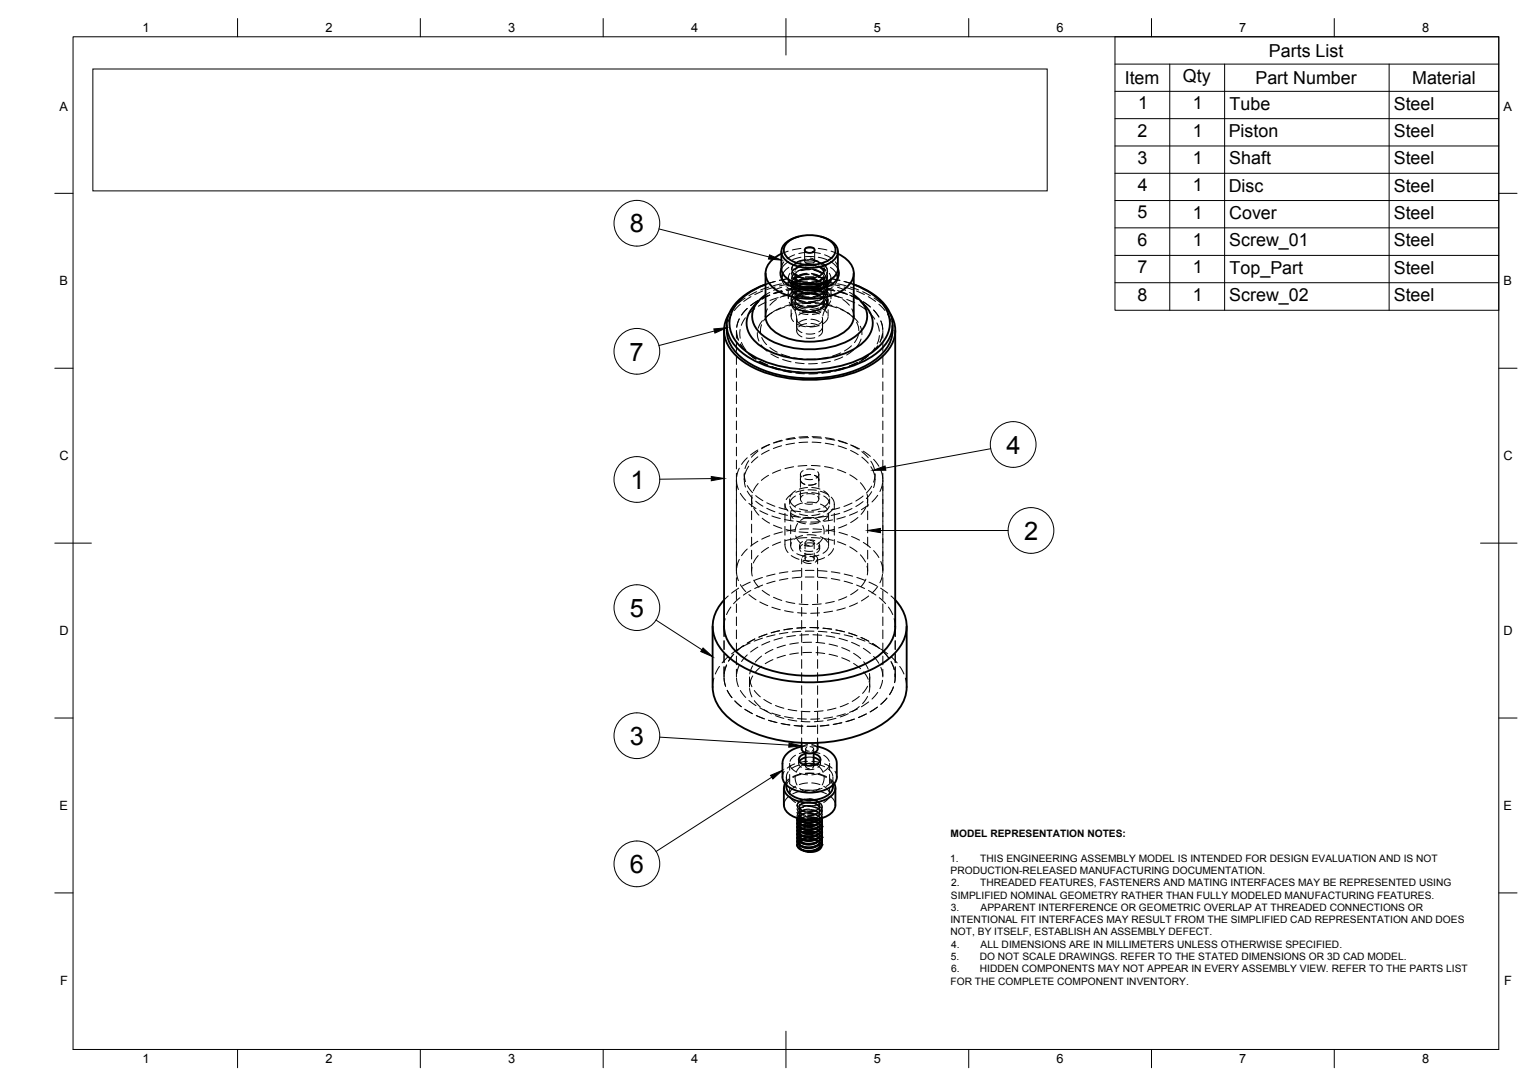
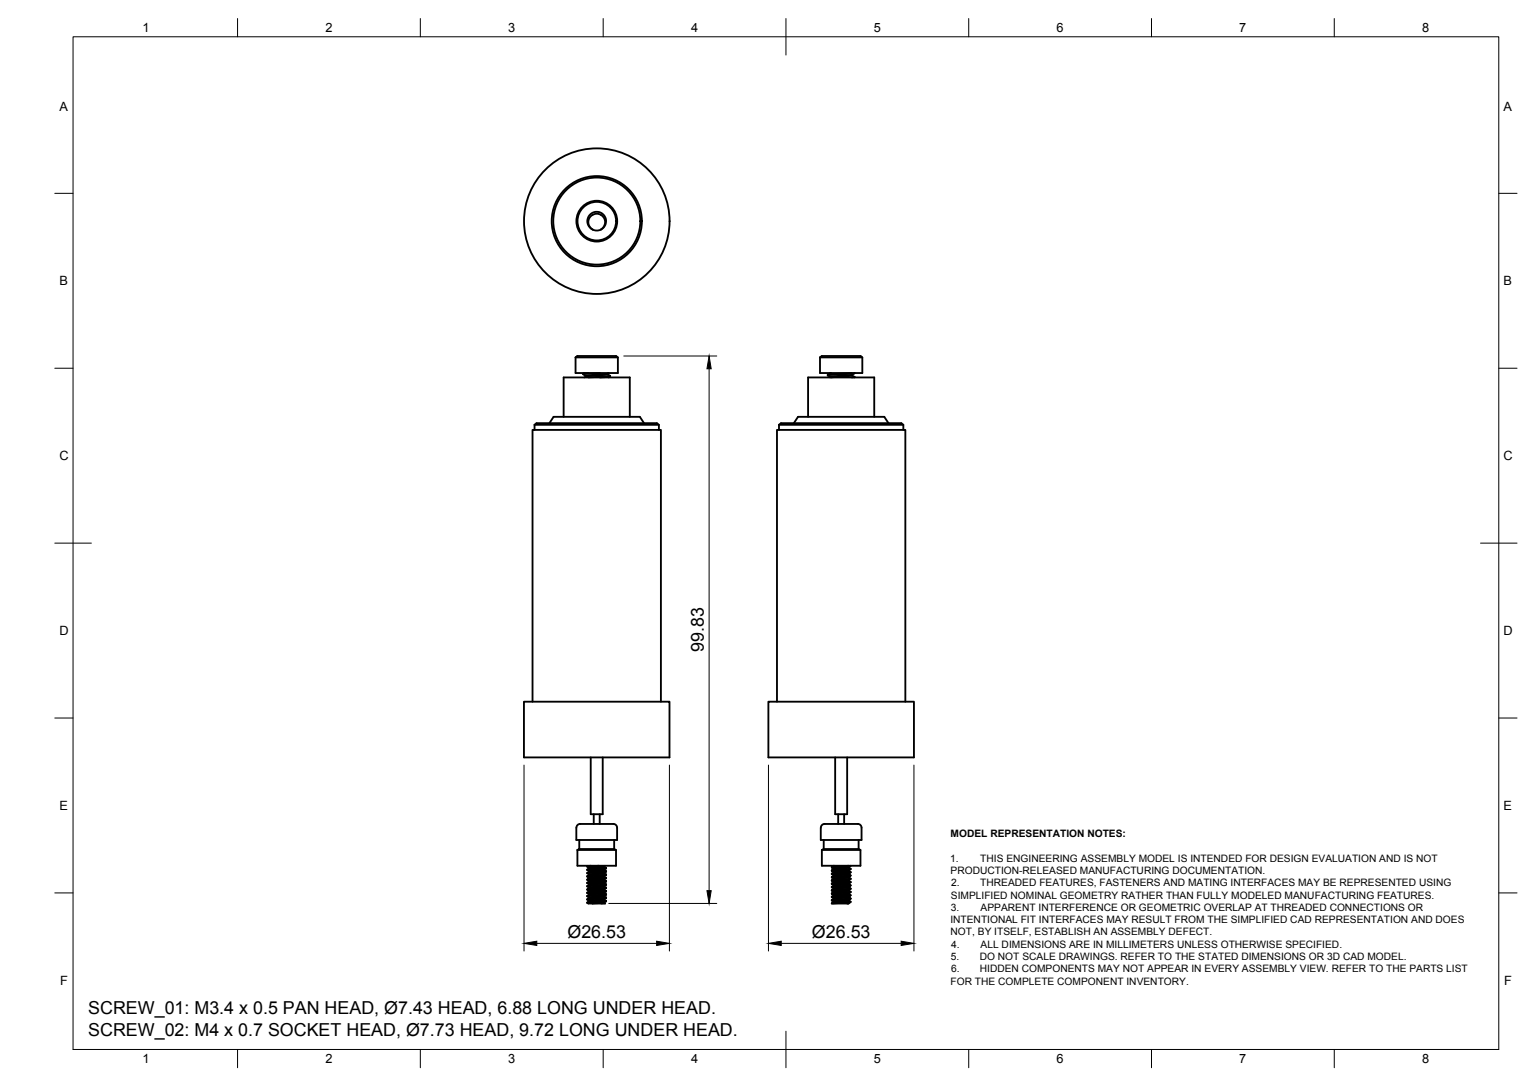
ISO-10303-21;
HEADER;
/* Generated by software containing ST-Developer
 * from STEP Tools, Inc. (www.steptools.com) 
 */

FILE_DESCRIPTION(
/* description */ (''),
/* implementation_level */ '2;1');

FILE_NAME(
/* name */ 'BR-113',
/* time_stamp */ '2026-10-04T22:56:18-07:00',
/* author */ (''),
/* organization */ (''),
/* preprocessor_version */ 'ST-DEVELOPER v20.2',
/* originating_system */ 'Autodesk Translation Framework v15.15.0.0',
/* authorisation */ '');

FILE_SCHEMA (('AUTOMOTIVE_DESIGN { 1 0 10303 214 3 1 1 }'));
ENDSEC;

DATA;
#10=MECHANICAL_DESIGN_GEOMETRIC_PRESENTATION_REPRESENTATION('',(#190,#191,
#192,#193,#194,#195,#196,#197),#14544);
#11=ITEM_DEFINED_TRANSFORMATION($,$,#1924,#2120);
#12=ITEM_DEFINED_TRANSFORMATION($,$,#1933,#2121);
#13=ITEM_DEFINED_TRANSFORMATION($,$,#1966,#2122);
#14=ITEM_DEFINED_TRANSFORMATION($,$,#1982,#2123);
#15=ITEM_DEFINED_TRANSFORMATION($,$,#1991,#2124);
#16=ITEM_DEFINED_TRANSFORMATION($,$,#2004,#2125);
#17=ITEM_DEFINED_TRANSFORMATION($,$,#2047,#2126);
#18=ITEM_DEFINED_TRANSFORMATION($,$,#2086,#2127);
#19=(
REPRESENTATION_RELATIONSHIP($,$,#14576,#14575)
REPRESENTATION_RELATIONSHIP_WITH_TRANSFORMATION(#11)
SHAPE_REPRESENTATION_RELATIONSHIP()
);
#20=(
REPRESENTATION_RELATIONSHIP($,$,#14577,#14575)
REPRESENTATION_RELATIONSHIP_WITH_TRANSFORMATION(#12)
SHAPE_REPRESENTATION_RELATIONSHIP()
);
#21=(
REPRESENTATION_RELATIONSHIP($,$,#14578,#14575)
REPRESENTATION_RELATIONSHIP_WITH_TRANSFORMATION(#13)
SHAPE_REPRESENTATION_RELATIONSHIP()
);
#22=(
REPRESENTATION_RELATIONSHIP($,$,#14579,#14575)
REPRESENTATION_RELATIONSHIP_WITH_TRANSFORMATION(#14)
SHAPE_REPRESENTATION_RELATIONSHIP()
);
#23=(
REPRESENTATION_RELATIONSHIP($,$,#14580,#14575)
REPRESENTATION_RELATIONSHIP_WITH_TRANSFORMATION(#15)
SHAPE_REPRESENTATION_RELATIONSHIP()
);
#24=(
REPRESENTATION_RELATIONSHIP($,$,#14581,#14575)
REPRESENTATION_RELATIONSHIP_WITH_TRANSFORMATION(#16)
SHAPE_REPRESENTATION_RELATIONSHIP()
);
#25=(
REPRESENTATION_RELATIONSHIP($,$,#14582,#14575)
REPRESENTATION_RELATIONSHIP_WITH_TRANSFORMATION(#17)
SHAPE_REPRESENTATION_RELATIONSHIP()
);
#26=(
REPRESENTATION_RELATIONSHIP($,$,#14583,#14575)
REPRESENTATION_RELATIONSHIP_WITH_TRANSFORMATION(#18)
SHAPE_REPRESENTATION_RELATIONSHIP()
);
#27=CONTEXT_DEPENDENT_SHAPE_REPRESENTATION(#19,#14567);
#28=CONTEXT_DEPENDENT_SHAPE_REPRESENTATION(#20,#14568);
#29=CONTEXT_DEPENDENT_SHAPE_REPRESENTATION(#21,#14569);
#30=CONTEXT_DEPENDENT_SHAPE_REPRESENTATION(#22,#14570);
#31=CONTEXT_DEPENDENT_SHAPE_REPRESENTATION(#23,#14571);
#32=CONTEXT_DEPENDENT_SHAPE_REPRESENTATION(#24,#14572);
#33=CONTEXT_DEPENDENT_SHAPE_REPRESENTATION(#25,#14573);
#34=CONTEXT_DEPENDENT_SHAPE_REPRESENTATION(#26,#14574);
#35=NEXT_ASSEMBLY_USAGE_OCCURRENCE('Tube:1','Tube:1','Tube:1',#14585,#14586,
'Tube:1');
#36=NEXT_ASSEMBLY_USAGE_OCCURRENCE('Piston:1','Piston:1','Piston:1',#14585,
#14587,'Piston:1');
#37=NEXT_ASSEMBLY_USAGE_OCCURRENCE('Shaft:1','Shaft:1','Shaft:1',#14585,
#14588,'Shaft:1');
#38=NEXT_ASSEMBLY_USAGE_OCCURRENCE('Disc:1','Disc:1','Disc:1',#14585,#14589,
'Disc:1');
#39=NEXT_ASSEMBLY_USAGE_OCCURRENCE('Cover:1','Cover:1','Cover:1',#14585,
#14590,'Cover:1');
#40=NEXT_ASSEMBLY_USAGE_OCCURRENCE('Screw_01:1','Screw_01:1',
'Screw_01:1',#14585,#14591,'Screw_01:1');
#41=NEXT_ASSEMBLY_USAGE_OCCURRENCE('Top_Part:1','Top_Part:1',
'Top_Part:1',#14585,#14592,'Top_Part:1');
#42=NEXT_ASSEMBLY_USAGE_OCCURRENCE('Screw_02:1','Screw_02:1',
'Screw_02:1',#14585,#14593,'Screw_02:1');
#43=CONICAL_SURFACE('',#2029,3.34979916874976,1.09810780243133);
#44=CONICAL_SURFACE('',#2051,6.94221583892671,0.735432745767903);
#45=CONICAL_SURFACE('',#2055,9.77637943942299,0.712897062744303);
#46=CONICAL_SURFACE('',#2061,11.1537701181833,0.893668754257897);
#47=CONICAL_SURFACE('',#2065,8.2465180845384,0.582247271411204);
#48=CONICAL_SURFACE('',#2073,3.90337928524842,0.252845151189765);
#49=CONICAL_SURFACE('',#2083,2.14952775522097,1.03539162387167);
#50=CONICAL_SURFACE('',#2110,3.70051543670999,0.906750163968186);
#51=B_SPLINE_SURFACE_WITH_KNOTS('',3,3,((#7599,#7600,#7601,#7602,#7603,
#7604,#7605,#7606,#7607,#7608,#7609,#7610,#7611,#7612,#7613,#7614,#7615,
#7616,#7617,#7618,#7619,#7620,#7621,#7622,#7623,#7624,#7625,#7626,#7627,
#7628,#7629,#7630,#7631,#7632,#7633,#7634,#7635,#7636,#7637,#7638,#7639,
#7640,#7641,#7642,#7643,#7644,#7645,#7646,#7647,#7648,#7649,#7650,#7651,
#7652,#7653,#7654,#7655,#7656,#7657,#7658,#7659,#7660,#7661,#7662,#7663,
#7664,#7665,#7666,#7667,#7668,#7669,#7670,#7671,#7672,#7673,#7674,#7675,
#7676),(#7677,#7678,#7679,#7680,#7681,#7682,#7683,#7684,#7685,#7686,#7687,
#7688,#7689,#7690,#7691,#7692,#7693,#7694,#7695,#7696,#7697,#7698,#7699,
#7700,#7701,#7702,#7703,#7704,#7705,#7706,#7707,#7708,#7709,#7710,#7711,
#7712,#7713,#7714,#7715,#7716,#7717,#7718,#7719,#7720,#7721,#7722,#7723,
#7724,#7725,#7726,#7727,#7728,#7729,#7730,#7731,#7732,#7733,#7734,#7735,
#7736,#7737,#7738,#7739,#7740,#7741,#7742,#7743,#7744,#7745,#7746,#7747,
#7748,#7749,#7750,#7751,#7752,#7753,#7754),(#7755,#7756,#7757,#7758,#7759,
#7760,#7761,#7762,#7763,#7764,#7765,#7766,#7767,#7768,#7769,#7770,#7771,
#7772,#7773,#7774,#7775,#7776,#7777,#7778,#7779,#7780,#7781,#7782,#7783,
#7784,#7785,#7786,#7787,#7788,#7789,#7790,#7791,#7792,#7793,#7794,#7795,
#7796,#7797,#7798,#7799,#7800,#7801,#7802,#7803,#7804,#7805,#7806,#7807,
#7808,#7809,#7810,#7811,#7812,#7813,#7814,#7815,#7816,#7817,#7818,#7819,
#7820,#7821,#7822,#7823,#7824,#7825,#7826,#7827,#7828,#7829,#7830,#7831,
#7832),(#7833,#7834,#7835,#7836,#7837,#7838,#7839,#7840,#7841,#7842,#7843,
#7844,#7845,#7846,#7847,#7848,#7849,#7850,#7851,#7852,#7853,#7854,#7855,
#7856,#7857,#7858,#7859,#7860,#7861,#7862,#7863,#7864,#7865,#7866,#7867,
#7868,#7869,#7870,#7871,#7872,#7873,#7874,#7875,#7876,#7877,#7878,#7879,
#7880,#7881,#7882,#7883,#7884,#7885,#7886,#7887,#7888,#7889,#7890,#7891,
#7892,#7893,#7894,#7895,#7896,#7897,#7898,#7899,#7900,#7901,#7902,#7903,
#7904,#7905,#7906,#7907,#7908,#7909,#7910)),.UNSPECIFIED.,.F.,.F.,.F.,(4,
4),(4,1,1,1,1,1,1,1,1,1,1,1,1,1,1,1,1,1,1,1,1,1,1,1,1,1,1,1,1,1,1,1,1,1,
1,1,1,1,1,1,1,1,1,1,1,1,1,1,1,1,1,1,1,1,1,1,1,1,1,1,1,1,1,1,1,1,1,1,1,1,
1,1,1,1,1,4),(-0.000270112238314874,0.0397652738162967),(8.3062683528249,
9.29465849132061,10.2830486298163,11.271438768312,12.2598289068078,13.2482190453035,
14.2366091837992,15.2249993222949,16.2133894607906,17.2017795992863,18.190169737782,
19.1785598762778,20.1669500147735,21.1553401532692,22.1437302917649,23.1321204302606,
24.1205105687563,25.108900707252,26.0972908457478,27.0856809842435,28.0740711227392,
29.0624612612349,30.0508513997306,31.0392415382263,32.027631676722,33.0160218152178,
34.0044119537135,34.9928020922092,35.9811922307049,36.9695823692006,37.9579725076963,
38.946362646192,39.9347527846878,40.9231429231835,41.9115330616792,42.8999232001749,
43.8883133386706,44.8767034771663,45.865093615662,46.8534837541578,47.8418738926535,
48.8302640311492,49.8186541696449,50.8070443081406,51.7954344466363,52.783824585132,
53.7722147236278,54.7606048621235,55.7489950006192,56.7373851391149,57.7257752776106,
58.7141654161063,59.702555554602,60.6909456930978,61.6793358315935,62.6677259700892,
63.6561161085849,64.6445062470806,65.6328963855763,66.621286524072,67.6096766625678,
68.5980668010635,69.5864569395592,70.5748470780549,71.5632372165506,72.5516273550463,
73.5400174935421,74.5284076320378,75.5167977705335,76.5051879090292,77.4935780475249,
78.4819681860206,79.4703583245163,80.458748463012,81.4471386015078,82.4357988522418),
 .UNSPECIFIED.);
#52=B_SPLINE_SURFACE_WITH_KNOTS('',3,3,((#8072,#8073,#8074,#8075,#8076,
#8077,#8078,#8079,#8080,#8081,#8082,#8083,#8084,#8085,#8086,#8087,#8088,
#8089,#8090,#8091,#8092,#8093,#8094,#8095,#8096,#8097,#8098,#8099,#8100,
#8101,#8102,#8103,#8104,#8105,#8106,#8107,#8108,#8109,#8110,#8111,#8112,
#8113,#8114,#8115,#8116,#8117,#8118,#8119,#8120,#8121,#8122,#8123,#8124,
#8125,#8126,#8127,#8128,#8129,#8130,#8131,#8132,#8133,#8134,#8135,#8136,
#8137,#8138,#8139,#8140,#8141,#8142,#8143,#8144,#8145,#8146,#8147,#8148,
#8149),(#8150,#8151,#8152,#8153,#8154,#8155,#8156,#8157,#8158,#8159,#8160,
#8161,#8162,#8163,#8164,#8165,#8166,#8167,#8168,#8169,#8170,#8171,#8172,
#8173,#8174,#8175,#8176,#8177,#8178,#8179,#8180,#8181,#8182,#8183,#8184,
#8185,#8186,#8187,#8188,#8189,#8190,#8191,#8192,#8193,#8194,#8195,#8196,
#8197,#8198,#8199,#8200,#8201,#8202,#8203,#8204,#8205,#8206,#8207,#8208,
#8209,#8210,#8211,#8212,#8213,#8214,#8215,#8216,#8217,#8218,#8219,#8220,
#8221,#8222,#8223,#8224,#8225,#8226,#8227),(#8228,#8229,#8230,#8231,#8232,
#8233,#8234,#8235,#8236,#8237,#8238,#8239,#8240,#8241,#8242,#8243,#8244,
#8245,#8246,#8247,#8248,#8249,#8250,#8251,#8252,#8253,#8254,#8255,#8256,
#8257,#8258,#8259,#8260,#8261,#8262,#8263,#8264,#8265,#8266,#8267,#8268,
#8269,#8270,#8271,#8272,#8273,#8274,#8275,#8276,#8277,#8278,#8279,#8280,
#8281,#8282,#8283,#8284,#8285,#8286,#8287,#8288,#8289,#8290,#8291,#8292,
#8293,#8294,#8295,#8296,#8297,#8298,#8299,#8300,#8301,#8302,#8303,#8304,
#8305),(#8306,#8307,#8308,#8309,#8310,#8311,#8312,#8313,#8314,#8315,#8316,
#8317,#8318,#8319,#8320,#8321,#8322,#8323,#8324,#8325,#8326,#8327,#8328,
#8329,#8330,#8331,#8332,#8333,#8334,#8335,#8336,#8337,#8338,#8339,#8340,
#8341,#8342,#8343,#8344,#8345,#8346,#8347,#8348,#8349,#8350,#8351,#8352,
#8353,#8354,#8355,#8356,#8357,#8358,#8359,#8360,#8361,#8362,#8363,#8364,
#8365,#8366,#8367,#8368,#8369,#8370,#8371,#8372,#8373,#8374,#8375,#8376,
#8377,#8378,#8379,#8380,#8381,#8382,#8383)),.UNSPECIFIED.,.F.,.F.,.F.,(4,
4),(4,1,1,1,1,1,1,1,1,1,1,1,1,1,1,1,1,1,1,1,1,1,1,1,1,1,1,1,1,1,1,1,1,1,
1,1,1,1,1,1,1,1,1,1,1,1,1,1,1,1,1,1,1,1,1,1,1,1,1,1,1,1,1,1,1,1,1,1,1,1,
1,1,1,1,1,4),(-0.000234520548766864,0.0397897202828816),(11.6153673532494,
12.6040275861021,13.5924177245978,14.5808078630935,15.5691980015892,16.5575881400849,
17.5459782785806,18.5343684170764,19.5227585555721,20.5111486940678,21.4995388325635,
22.4879289710592,23.4763191095549,24.4647092480506,25.4530993865464,26.4414895250421,
27.4298796635378,28.4182698020335,29.4066599405292,30.3950500790249,31.3834402175206,
32.3718303560164,33.3602204945121,34.3486106330078,35.3370007715035,36.3253909099992,
37.3137810484949,38.3021711869906,39.2905613254864,40.2789514639821,41.2673416024778,
42.2557317409735,43.2441218794692,44.2325120179649,45.2209021564607,46.2092922949564,
47.1976824334521,48.1860725719478,49.1744627104435,50.1628528489392,51.1512429874349,
52.1396331259307,53.1280232644264,54.1164134029221,55.1048035414178,56.0931936799135,
57.0815838184092,58.0699739569049,59.0583640954007,60.0467542338964,61.0351443723921,
62.0235345108878,63.0119246493835,64.0003147878792,64.988704926375,65.9770950648707,
66.9654852033664,67.9538753418621,68.9422654803578,69.9306556188535,70.9190457573492,
71.907435895845,72.8958260343407,73.8842161728364,74.8726063113321,75.8609964498278,
76.8493865883235,77.8377767268192,78.8261668653149,79.8145570038107,80.8029471423064,
81.7913372808021,82.7797274192978,83.7681175577935,84.7565076962892,85.7449775254208),
 .UNSPECIFIED.);
#53=B_SPLINE_SURFACE_WITH_KNOTS('',3,3,((#13719,#13720,#13721,#13722,#13723,
#13724,#13725,#13726,#13727,#13728,#13729,#13730,#13731,#13732,#13733,#13734,
#13735,#13736,#13737,#13738,#13739,#13740,#13741,#13742,#13743,#13744,#13745,
#13746,#13747,#13748,#13749,#13750,#13751,#13752,#13753,#13754,#13755,#13756,
#13757,#13758,#13759,#13760,#13761,#13762,#13763,#13764,#13765,#13766,#13767,
#13768,#13769,#13770),(#13771,#13772,#13773,#13774,#13775,#13776,#13777,
#13778,#13779,#13780,#13781,#13782,#13783,#13784,#13785,#13786,#13787,#13788,
#13789,#13790,#13791,#13792,#13793,#13794,#13795,#13796,#13797,#13798,#13799,
#13800,#13801,#13802,#13803,#13804,#13805,#13806,#13807,#13808,#13809,#13810,
#13811,#13812,#13813,#13814,#13815,#13816,#13817,#13818,#13819,#13820,#13821,
#13822),(#13823,#13824,#13825,#13826,#13827,#13828,#13829,#13830,#13831,
#13832,#13833,#13834,#13835,#13836,#13837,#13838,#13839,#13840,#13841,#13842,
#13843,#13844,#13845,#13846,#13847,#13848,#13849,#13850,#13851,#13852,#13853,
#13854,#13855,#13856,#13857,#13858,#13859,#13860,#13861,#13862,#13863,#13864,
#13865,#13866,#13867,#13868,#13869,#13870,#13871,#13872,#13873,#13874),
(#13875,#13876,#13877,#13878,#13879,#13880,#13881,#13882,#13883,#13884,
#13885,#13886,#13887,#13888,#13889,#13890,#13891,#13892,#13893,#13894,#13895,
#13896,#13897,#13898,#13899,#13900,#13901,#13902,#13903,#13904,#13905,#13906,
#13907,#13908,#13909,#13910,#13911,#13912,#13913,#13914,#13915,#13916,#13917,
#13918,#13919,#13920,#13921,#13922,#13923,#13924,#13925,#13926)),
 .UNSPECIFIED.,.F.,.F.,.F.,(4,4),(4,1,1,1,1,1,1,1,1,1,1,1,1,1,1,1,1,1,1,
1,1,1,1,1,1,1,1,1,1,1,1,1,1,1,1,1,1,1,1,1,1,1,1,1,1,1,1,1,1,4),(-0.000425975868175074,
0.0530000950082445),(8.30815772716284,9.30770753701498,10.3072573468671,
11.3068071567193,12.3063569665714,13.3059067764236,14.3054565862757,15.3050063961278,
16.30455620598,17.3041060158321,18.3036558256843,19.3032056355364,20.3027554453886,
21.3023052552407,22.3018550650929,23.301404874945,24.3009546847971,25.3005044946493,
26.3000543045014,27.2996041143536,28.2991539242057,29.2987037340579,30.29825354391,
31.2978033537621,32.2973531636143,33.2969029734664,34.2964527833186,35.2960025931707,
36.2955524030229,37.295102212875,38.2946520227271,39.2942018325793,40.2937516424314,
41.2933014522836,42.2928512621357,43.2924010719879,44.29195088184,45.2915006916922,
46.2910505015443,47.2906003113964,48.2901501212486,49.2896999311007,50.2892497409529,
51.288799550805,52.2883493606572,53.2878991705093,54.2874489803615,55.2869987902136,
56.2865486000657,57.2865243857861),.UNSPECIFIED.);
#54=B_SPLINE_SURFACE_WITH_KNOTS('',3,3,((#14187,#14188,#14189,#14190,#14191,
#14192,#14193,#14194,#14195,#14196,#14197,#14198,#14199,#14200,#14201,#14202,
#14203,#14204,#14205,#14206,#14207,#14208,#14209,#14210,#14211,#14212,#14213,
#14214,#14215,#14216,#14217,#14218,#14219,#14220,#14221,#14222,#14223,#14224,
#14225,#14226,#14227,#14228,#14229,#14230,#14231,#14232,#14233,#14234,#14235,
#14236,#14237,#14238),(#14239,#14240,#14241,#14242,#14243,#14244,#14245,
#14246,#14247,#14248,#14249,#14250,#14251,#14252,#14253,#14254,#14255,#14256,
#14257,#14258,#14259,#14260,#14261,#14262,#14263,#14264,#14265,#14266,#14267,
#14268,#14269,#14270,#14271,#14272,#14273,#14274,#14275,#14276,#14277,#14278,
#14279,#14280,#14281,#14282,#14283,#14284,#14285,#14286,#14287,#14288,#14289,
#14290),(#14291,#14292,#14293,#14294,#14295,#14296,#14297,#14298,#14299,
#14300,#14301,#14302,#14303,#14304,#14305,#14306,#14307,#14308,#14309,#14310,
#14311,#14312,#14313,#14314,#14315,#14316,#14317,#14318,#14319,#14320,#14321,
#14322,#14323,#14324,#14325,#14326,#14327,#14328,#14329,#14330,#14331,#14332,
#14333,#14334,#14335,#14336,#14337,#14338,#14339,#14340,#14341,#14342),
(#14343,#14344,#14345,#14346,#14347,#14348,#14349,#14350,#14351,#14352,
#14353,#14354,#14355,#14356,#14357,#14358,#14359,#14360,#14361,#14362,#14363,
#14364,#14365,#14366,#14367,#14368,#14369,#14370,#14371,#14372,#14373,#14374,
#14375,#14376,#14377,#14378,#14379,#14380,#14381,#14382,#14383,#14384,#14385,
#14386,#14387,#14388,#14389,#14390,#14391,#14392,#14393,#14394)),
 .UNSPECIFIED.,.F.,.F.,.F.,(4,4),(4,1,1,1,1,1,1,1,1,1,1,1,1,1,1,1,1,1,1,
1,1,1,1,1,1,1,1,1,1,1,1,1,1,1,1,1,1,1,1,1,1,1,1,1,1,1,1,1,1,4),(-0.000359185103406873,
0.0530514251731689),(11.6159672492052,12.6159430071938,13.615492817046,
14.6150426268981,15.6145924367503,16.6141422466024,17.6136920564545,18.6132418663067,
19.6127916761588,20.612341486011,21.6118912958631,22.6114411057153,23.6109909155674,
24.6105407254196,25.6100905352717,26.6096403451238,27.609190154976,28.6087399648281,
29.6082897746803,30.6078395845324,31.6073893943846,32.6069392042367,33.6064890140888,
34.606038823941,35.6055886337931,36.6051384436453,37.6046882534974,38.6042380633496,
39.6037878732017,40.6033376830538,41.602887492906,42.6024373027581,43.6019871126103,
44.6015369224624,45.6010867323146,46.6006365421667,47.6001863520188,48.599736161871,
49.5992859717231,50.5988357815753,51.5983855914274,52.5979354012796,53.5974852111317,
54.5970350209839,55.596584830836,56.5961346406881,57.5956844505403,58.5952342603924,
59.5947840702446,60.5943338800967),.UNSPECIFIED.);
#55=B_SPLINE_CURVE_WITH_KNOTS('',3,(#2735,#2736,#2737,#2738,#2739,#2740,
#2741,#2742,#2743,#2744,#2745,#2746,#2747,#2748,#2749,#2750,#2751,#2752,
#2753,#2754,#2755,#2756,#2757,#2758,#2759,#2760,#2761,#2762,#2763,#2764,
#2765,#2766,#2767,#2768,#2769,#2770,#2771,#2772,#2773,#2774,#2775,#2776,
#2777,#2778,#2779,#2780,#2781,#2782,#2783,#2784,#2785,#2786,#2787,#2788,
#2789,#2790,#2791,#2792,#2793,#2794,#2795,#2796,#2797,#2798,#2799,#2800,
#2801,#2802,#2803,#2804,#2805,#2806,#2807,#2808,#2809,#2810,#2811,#2812,
#2813,#2814,#2815,#2816,#2817,#2818,#2819,#2820,#2821,#2822,#2823,#2824,
#2825,#2826,#2827,#2828,#2829,#2830,#2831,#2832,#2833,#2834,#2835,#2836,
#2837,#2838,#2839,#2840,#2841,#2842,#2843,#2844,#2845,#2846,#2847,#2848,
#2849,#2850,#2851,#2852,#2853,#2854,#2855,#2856,#2857,#2858,#2859,#2860,
#2861,#2862,#2863,#2864),.UNSPECIFIED.,.F.,.F.,(4,3,3,3,3,3,3,3,3,3,3,3,
3,3,3,3,3,3,3,3,3,3,3,3,3,3,3,3,3,3,3,3,3,3,3,3,3,3,3,3,3,3,3,4),(10.3759830427441,
10.4901328275944,10.6041362297079,10.7180425069784,10.8319007590481,10.945840293292,
11.059816326816,11.1740039201576,11.271438768312,11.3871452657409,11.5026525812533,
11.6180501086129,11.7333845017257,11.8487023154049,11.9641311047711,12.0796198011564,
12.1953197159756,12.2598289068078,12.3751876429801,12.4903373625612,12.605371537628,
12.7203375249411,12.8352825749272,12.9503349124734,13.0654445419192,13.1807657388827,
13.2482190453035,13.3637725587923,13.4791207741952,13.5943555713228,13.7095239270441,
13.8246727146767,13.9399292713301,14.0552436848736,14.1707681415781,14.2366091837992,
14.3521052552483,14.4674378367289,14.5826541109109,14.6978010922988,14.8129875625007,
14.9281889246498,15.0435538422179,15.1339731442208),.UNSPECIFIED.);
#56=B_SPLINE_CURVE_WITH_KNOTS('',3,(#2867,#2868,#2869,#2870,#2871,#2872,
#2873,#2874,#2875,#2876,#2877,#2878,#2879,#2880,#2881,#2882,#2883,#2884,
#2885,#2886,#2887,#2888,#2889,#2890,#2891,#2892,#2893,#2894,#2895,#2896,
#2897,#2898,#2899,#2900,#2901,#2902,#2903,#2904,#2905,#2906,#2907,#2908,
#2909,#2910,#2911,#2912,#2913,#2914,#2915,#2916,#2917,#2918,#2919,#2920,
#2921,#2922,#2923,#2924,#2925,#2926,#2927,#2928,#2929,#2930,#2931,#2932,
#2933,#2934,#2935,#2936,#2937,#2938,#2939,#2940,#2941,#2942,#2943,#2944,
#2945,#2946,#2947,#2948,#2949,#2950,#2951,#2952,#2953,#2954,#2955,#2956,
#2957,#2958,#2959,#2960,#2961,#2962,#2963),.UNSPECIFIED.,.F.,.F.,(4,3,3,
3,3,3,3,3,3,3,3,3,3,3,3,3,3,3,3,3,3,3,3,3,3,3,3,3,3,3,3,3,4),(11.6156374476063,
11.7391862149183,11.8573028306364,11.9753941171691,12.0934978467133,12.2116517975586,
12.329985894632,12.4484221855639,12.5670917656992,12.6040275861021,12.7183681437411,
12.8324766304615,12.9464559897273,13.0603553078476,13.1742235395948,13.2881915462384,
13.4022107702393,13.5164447310029,13.5924177245978,13.7081224421998,13.8236218489584,
13.9390076808891,14.0543266075558,14.1696251946564,14.2850291383448,14.4004897681705,
14.5161568443809,14.5808078630935,14.6965062137723,14.8120136139633,14.9274078470399,
15.0427609094787,15.1341554268676),.UNSPECIFIED.);
#57=B_SPLINE_CURVE_WITH_KNOTS('',3,(#2969,#2970,#2971,#2972,#2973,#2974,
#2975,#2976,#2977,#2978,#2979,#2980,#2981,#2982,#2983,#2984,#2985,#2986,
#2987,#2988,#2989,#2990,#2991,#2992,#2993,#2994,#2995,#2996,#2997,#2998,
#2999,#3000,#3001,#3002,#3003,#3004,#3005,#3006,#3007,#3008,#3009,#3010,
#3011,#3012,#3013,#3014,#3015,#3016,#3017,#3018,#3019,#3020,#3021,#3022,
#3023,#3024,#3025,#3026,#3027,#3028,#3029,#3030,#3031,#3032,#3033,#3034,
#3035,#3036,#3037,#3038,#3039,#3040,#3041,#3042,#3043,#3044,#3045,#3046,
#3047,#3048,#3049,#3050,#3051,#3052,#3053,#3054,#3055,#3056,#3057,#3058,
#3059,#3060,#3061,#3062,#3063,#3064,#3065,#3066,#3067,#3068,#3069,#3070,
#3071,#3072,#3073,#3074,#3075,#3076,#3077,#3078,#3079,#3080,#3081,#3082,
#3083,#3084,#3085,#3086,#3087,#3088,#3089,#3090,#3091,#3092,#3093,#3094,
#3095,#3096,#3097,#3098,#3099,#3100,#3101,#3102,#3103,#3104,#3105,#3106,
#3107,#3108,#3109,#3110,#3111,#3112,#3113,#3114,#3115,#3116,#3117,#3118,
#3119,#3120,#3121,#3122,#3123,#3124,#3125,#3126,#3127,#3128,#3129,#3130),
 .UNSPECIFIED.,.F.,.F.,(4,2,2,2,2,2,2,2,2,2,2,2,2,2,2,2,2,2,2,2,2,2,2,2,
2,2,2,2,2,2,2,2,2,2,2,2,2,2,2,2,2,2,2,2,2,2,2,2,2,2,2,2,2,2,2,2,2,2,2,2,
2,2,2,2,2,2,2,2,2,2,2,2,2,2,2,2,2,2,2,2,4),(-0.782733604482233,-0.770157826719555,
-0.75276206461562,-0.749117370176853,-0.746928419369716,-0.744809097682532,
-0.741494339600281,-0.729784458095009,-0.699450263751413,-0.687219107000443,
-0.682196332555423,-0.678553517357403,-0.674699027671161,-0.668554315985148,
-0.643216717155835,-0.618451838435992,-0.614233101788583,-0.611898861798471,
-0.60985120678557,-0.606936417014568,-0.599096973822123,-0.585625401079225,
-0.554603092751879,-0.548267267232944,-0.544373902366787,-0.54074736296389,
-0.535831177246758,-0.52348909216597,-0.502676938067557,-0.482047164365493,
-0.478333961048462,-0.476130270859124,-0.474021706684097,-0.470760189917674,
-0.459690893796215,-0.433537235515639,-0.417340314888203,-0.411904812651969,
-0.40856057787087,-0.404881436392131,-0.399643933838947,-0.384522469156377,
-0.351092146048453,-0.344691775828512,-0.342166120108992,-0.340124695693966,
-0.337840686644481,-0.333745862398689,-0.328456060128697,-0.315438052231705,
-0.283483619822755,-0.277271769532392,-0.27340351470766,-0.269766608754107,
-0.26478253529075,-0.251911110080875,-0.23086309942583,-0.21262219916004,
-0.208132631152173,-0.20574057158714,-0.203910420600591,-0.201234128576658,
-0.195031417186624,-0.155419068666847,-0.144854541725996,-0.14013624586591,
-0.136525144863413,-0.132582005105212,-0.126004554399748,-0.105669836784276,
-0.0827148084467963,-0.07441218539548,-0.0713588103952259,-0.069309766435704,
-0.0670468362556635,-0.0630459662546947,-0.0419052067838259,-0.0135949473602621,
-0.00699940792823476,-0.00321792908897172,-0.000389459724301548),
 .UNSPECIFIED.);
#58=B_SPLINE_CURVE_WITH_KNOTS('',3,(#3131,#3132,#3133,#3134,#3135,#3136,
#3137,#3138,#3139,#3140,#3141,#3142,#3143,#3144,#3145,#3146),
 .UNSPECIFIED.,.F.,.F.,(4,3,3,3,3,4),(15.1339731442208,15.2249993222949,
15.3467969573775,15.4683336435129,15.5895226840091,15.707963267538),
 .UNSPECIFIED.);
#59=B_SPLINE_CURVE_WITH_KNOTS('',3,(#3148,#3149,#3150,#3151,#3152,#3153,
#3154,#3155,#3156,#3157,#3158,#3159,#3160,#3161,#3162,#3163),
 .UNSPECIFIED.,.F.,.F.,(4,3,3,3,3,4),(15.1341554268676,15.2495770896519,
15.3650499947019,15.4807417632621,15.5691980015892,15.7079632679489),
 .UNSPECIFIED.);
#60=B_SPLINE_CURVE_WITH_KNOTS('',3,(#3164,#3165,#3166,#3167,#3168,#3169,
#3170,#3171,#3172),.UNSPECIFIED.,.F.,.F.,(4,1,1,1,1,1,4),(15.7079705185665,
16.5575881400849,17.5459782785806,18.5343684170764,19.5227585555721,20.5111486940678,
21.4170854462023),.UNSPECIFIED.);
#61=B_SPLINE_CURVE_WITH_KNOTS('',3,(#3177,#3178,#3179,#3180,#3181,#3182,
#3183,#3184,#3185,#3186,#3187,#3188,#3189,#3190,#3191,#3192,#3193,#3194,
#3195,#3196,#3197,#3198,#3199,#3200,#3201,#3202,#3203,#3204,#3205,#3206,
#3207,#3208,#3209,#3210,#3211,#3212,#3213,#3214,#3215,#3216,#3217,#3218,
#3219,#3220,#3221,#3222,#3223,#3224,#3225,#3226,#3227,#3228,#3229,#3230,
#3231,#3232,#3233,#3234,#3235,#3236,#3237,#3238,#3239,#3240,#3241,#3242,
#3243,#3244,#3245,#3246,#3247,#3248,#3249,#3250,#3251,#3252,#3253,#3254,
#3255,#3256,#3257,#3258,#3259,#3260,#3261,#3262,#3263,#3264,#3265,#3266,
#3267,#3268,#3269,#3270,#3271,#3272,#3273,#3274,#3275,#3276,#3277,#3278,
#3279,#3280,#3281,#3282,#3283,#3284,#3285,#3286,#3287,#3288,#3289,#3290,
#3291,#3292,#3293,#3294,#3295,#3296,#3297,#3298,#3299,#3300,#3301,#3302,
#3303,#3304,#3305,#3306,#3307,#3308,#3309,#3310,#3311,#3312,#3313,#3314,
#3315,#3316,#3317,#3318,#3319,#3320,#3321,#3322,#3323,#3324,#3325,#3326,
#3327,#3328,#3329,#3330,#3331,#3332,#3333,#3334,#3335,#3336,#3337,#3338,
#3339,#3340,#3341,#3342,#3343,#3344,#3345,#3346,#3347,#3348,#3349,#3350,
#3351,#3352,#3353,#3354,#3355,#3356,#3357,#3358,#3359,#3360,#3361,#3362,
#3363,#3364,#3365,#3366,#3367,#3368),.UNSPECIFIED.,.F.,.F.,(4,2,2,2,2,2,
2,2,2,2,2,2,2,2,2,2,2,2,2,2,2,2,2,2,2,2,2,2,2,2,2,2,2,2,2,2,2,2,2,2,2,2,
2,2,2,2,2,2,2,2,2,2,2,2,2,2,2,2,2,2,2,2,2,2,2,2,2,2,2,2,2,2,2,2,2,2,2,2,
2,2,2,2,2,2,2,2,2,2,2,2,2,2,2,2,2,4),(-1.64352268459931,-1.63476883123318,
-1.63402567322011,-1.63342722906353,-1.63292767441782,-1.63249448823608,
-1.63210359140578,-1.63173566873332,-1.62780587104402,-1.62419491063142,
-1.61945946059501,-1.60875406191175,-1.5692722504643,-1.5630868427994,-1.56041499772771,
-1.55858668142764,-1.55619511324214,-1.55170442358894,-1.53342756718608,
-1.51705128748056,-1.50592128959387,-1.49762536274893,-1.49334906035993,
-1.4897823637737,-1.48548962780102,-1.47736787756967,-1.44698876904348,
-1.43527580264051,-1.42809762035076,-1.42527413818368,-1.42323930798832,
-1.42085734706968,-1.41641262574429,-1.39903345895037,-1.37692223120475,
-1.36418266009999,-1.35921637524091,-1.35558312958256,-1.35171026497336,
-1.34547166682427,-1.31371775484136,-1.30060020677027,-1.2928893692202,
-1.28999220021456,-1.2879476520995,-1.28560577432011,-1.28134973805828,
-1.25735089556425,-1.23089283838892,-1.22498034484753,-1.22117299188316,
-1.21754720293339,-1.21320927324726,-1.20251111723102,-1.16307507571946,
-1.15689929284964,-1.15422874640166,-1.15240033106973,-1.15000720512386,
-1.14551018571139,-1.12715260273344,-1.11038923180556,-1.09423498228552,
-1.08889918402023,-1.08520242147841,-1.08143559157495,-1.07573053130373,
-1.05538329047308,-1.02661649144373,-1.02116808771719,-1.01862165983652,
-1.01680350549185,-1.01431190689201,-1.00916448883525,-0.983352029504981,
-0.96760342616325,-0.957126394053837,-0.952478022594186,-0.948887423589241,
-0.944871769636762,-0.937927475085164,-0.90016904700671,-0.887657233503014,
-0.884281596906025,-0.882149647187371,-0.879975814846629,-0.876402543393401,
-0.861433002233763,-0.827960396031091,-0.820971161790752,-0.816561960136959,
-0.812991188864477,-0.80881638959142,-0.801062101183388,-0.785939975109009,
-0.782733604482233),.UNSPECIFIED.);
#62=B_SPLINE_CURVE_WITH_KNOTS('',3,(#3370,#3371,#3372,#3373,#3374),
 .UNSPECIFIED.,.F.,.F.,(4,1,4),(21.4170854462023,21.4995388325635,21.9911484110583),
 .UNSPECIFIED.);
#63=B_SPLINE_CURVE_WITH_KNOTS('',3,(#3375,#3376,#3377,#3378,#3379,#3380,
#3381,#3382,#3383,#3384,#3385,#3386,#3387,#3388,#3389,#3390,#3391,#3392,
#3393,#3394,#3395,#3396,#3397,#3398,#3399,#3400,#3401,#3402,#3403,#3404,
#3405,#3406,#3407,#3408,#3409,#3410,#3411,#3412,#3413,#3414,#3415,#3416,
#3417,#3418,#3419,#3420,#3421,#3422,#3423,#3424,#3425,#3426,#3427,#3428,
#3429,#3430,#3431,#3432,#3433,#3434,#3435,#3436,#3437,#3438,#3439,#3440,
#3441,#3442,#3443,#3444,#3445,#3446,#3447,#3448,#3449,#3450,#3451,#3452,
#3453,#3454,#3455,#3456,#3457,#3458,#3459,#3460,#3461,#3462,#3463,#3464,
#3465,#3466,#3467,#3468,#3469,#3470,#3471,#3472,#3473,#3474,#3475,#3476,
#3477,#3478,#3479,#3480,#3481,#3482,#3483,#3484,#3485,#3486,#3487,#3488,
#3489,#3490,#3491,#3492,#3493,#3494,#3495,#3496,#3497,#3498,#3499,#3500,
#3501,#3502,#3503,#3504,#3505,#3506,#3507,#3508,#3509,#3510,#3511,#3512,
#3513,#3514,#3515,#3516,#3517,#3518,#3519,#3520,#3521,#3522,#3523,#3524,
#3525,#3526,#3527,#3528,#3529,#3530,#3531,#3532,#3533,#3534,#3535,#3536,
#3537,#3538,#3539,#3540),.UNSPECIFIED.,.F.,.F.,(4,2,2,2,2,2,2,2,2,2,2,2,
2,2,2,2,2,2,2,2,2,2,2,2,2,2,2,2,2,2,2,2,2,2,2,2,2,2,2,2,2,2,2,2,2,2,2,2,
2,2,2,2,2,2,2,2,2,2,2,2,2,2,2,2,2,2,2,2,2,2,2,2,2,2,2,2,2,2,2,2,2,2,4),
(-1.72167836190146,-1.71993697657055,-1.71759155374419,-1.71275393978564,
-1.69882493517257,-1.66371621695858,-1.65747769739599,-1.6547979341954,
-1.65296929384515,-1.65058468672109,-1.64612528794294,-1.62511269287794,
-1.60556984059511,-1.59365078975702,-1.58879339412367,-1.58517730292486,
-1.58126424068391,-1.57482320787054,-1.5446452837465,-1.53072619827246,
-1.5227305689983,-1.51979650989599,-1.51774702764271,-1.51542452751536,
-1.51125629876888,-1.48585371079696,-1.46889497034311,-1.45792728782081,
-1.45320590782008,-1.44960839891158,-1.44563451111625,-1.43889109860587,
-1.41339125332872,-1.39655335652045,-1.38762130909995,-1.38457395257359,
-1.38250630070754,-1.38023319674731,-1.37618651598821,-1.34924651957977,
-1.3330791763852,-1.32571908232761,-1.31959747558421,-1.31574921255501,
-1.31210671097212,-1.3070753685696,-1.29477440026756,-1.26451274654844,
-1.25281244979044,-1.24949948968538,-1.24738135437933,-1.24519366027113,
-1.24155138653956,-1.22417074368823,-1.20840430116804,-1.19554919003907,
-1.18638082906214,-1.18194887606309,-1.17837865509488,-1.17422580645375,
-1.16679565946455,-1.12996502559649,-1.11753613239243,-1.1141675860736,
-1.11203782863533,-1.10986385442139,-1.10628663816915,-1.09120189733225,
-1.06618465948351,-1.05265511829926,-1.04759291403465,-1.04394490788819,
-1.04010573458198,-1.0340315116068,-1.00113166622705,-0.988561855242318,
-0.983380941651227,-0.979350457118574,-0.977080447749138,-0.975034464511672,
-0.972486208839398,-0.965923306996879,-0.939600795071122),.UNSPECIFIED.);
#64=B_SPLINE_CURVE_WITH_KNOTS('',3,(#3546,#3547,#3548,#3549,#3550,#3551,
#3552,#3553,#3554,#3555,#3556,#3557,#3558,#3559,#3560,#3561,#3562,#3563,
#3564,#3565,#3566,#3567,#3568,#3569,#3570,#3571,#3572,#3573,#3574,#3575,
#3576,#3577,#3578,#3579,#3580,#3581,#3582,#3583,#3584,#3585,#3586,#3587,
#3588,#3589,#3590,#3591,#3592,#3593,#3594,#3595,#3596,#3597,#3598,#3599,
#3600,#3601,#3602,#3603,#3604,#3605,#3606,#3607,#3608,#3609,#3610,#3611,
#3612,#3613,#3614,#3615,#3616,#3617,#3618,#3619,#3620,#3621,#3622,#3623,
#3624,#3625,#3626,#3627,#3628,#3629,#3630,#3631,#3632,#3633,#3634,#3635,
#3636,#3637,#3638,#3639,#3640,#3641,#3642,#3643,#3644,#3645,#3646,#3647,
#3648,#3649,#3650,#3651,#3652,#3653,#3654,#3655,#3656,#3657,#3658,#3659,
#3660,#3661,#3662,#3663,#3664,#3665,#3666,#3667,#3668,#3669,#3670,#3671,
#3672,#3673,#3674,#3675,#3676,#3677,#3678,#3679,#3680,#3681,#3682,#3683,
#3684,#3685,#3686,#3687,#3688,#3689,#3690,#3691,#3692,#3693,#3694,#3695,
#3696,#3697,#3698,#3699,#3700,#3701,#3702,#3703,#3704,#3705,#3706,#3707),
 .UNSPECIFIED.,.F.,.F.,(4,2,2,2,2,2,2,2,2,2,2,2,2,2,2,2,2,2,2,2,2,2,2,2,
2,2,2,2,2,2,2,2,2,2,2,2,2,2,2,2,2,2,2,2,2,2,2,2,2,2,2,2,2,2,2,2,2,2,2,2,
2,2,2,2,2,2,2,2,2,2,2,2,2,2,2,2,2,2,2,2,4),(-0.782696160082662,-0.781075359436944,
-0.77328328598361,-0.759943173937005,-0.728660283751481,-0.722359348904134,
-0.718473432435426,-0.714844722566713,-0.709911259337837,-0.697433398901302,
-0.676189046787961,-0.657661695477911,-0.653151516600006,-0.650755543412031,
-0.64892740805726,-0.646260580729097,-0.640108143481001,-0.600792497984823,
-0.590002994722619,-0.585651102005755,-0.582021754183454,-0.578219105711645,
-0.57233195335054,-0.565342597230487,-0.550560881162287,-0.527434583566802,
-0.519350947839438,-0.516327317227424,-0.514283286352171,-0.512006654137859,
-0.507946245131807,-0.502715089205647,-0.489938841318079,-0.457512448786117,
-0.451372549004067,-0.447519497986136,-0.443876944512898,-0.438852758095078,
-0.425649222564851,-0.406155914027626,-0.386778717188384,-0.382304629054381,
-0.37991643578708,-0.378087344850847,-0.375410016595597,-0.369191515686781,
-0.334159908112979,-0.320176506576414,-0.314947068059239,-0.31130634470972,
-0.307522347694134,-0.301727987493547,-0.277429585680445,-0.250569432024096,
-0.246508918257079,-0.244232316155977,-0.242164751680355,-0.239122043078044,
-0.230237091346038,-0.21356032098588,-0.187860668751238,-0.181119888635252,
-0.177145423124215,-0.173546012975649,-0.168820063054617,-0.157830956802909,
-0.140820171809713,-0.115418730256182,-0.111223191176004,-0.108918504830981,
-0.106861841514575,-0.10388561497163,-0.0955600489989513,-0.0806694248799056,
-0.0522417527946656,-0.0456226622466711,-0.0416726117827746,-0.038066367541658,
-0.0332884890336368,-0.0279803390021662,-0.000387520461421266),
 .UNSPECIFIED.);
#65=B_SPLINE_CURVE_WITH_KNOTS('',3,(#3708,#3709,#3710,#3711,#3712,#3713,
#3714,#3715,#3716,#3717,#3718,#3719,#3720,#3721,#3722,#3723,#3724,#3725,
#3726,#3727,#3728,#3729),.UNSPECIFIED.,.F.,.F.,(4,2,2,2,2,2,2,2,2,2,4),
(-1.72194463547043,-1.70657072393317,-1.70042690145371,-1.69777394834495,
-1.69578717472258,-1.69396043674524,-1.69156103513742,-1.68703187060117,
-1.66702483672176,-1.64687581390891,-1.64352268459931),.UNSPECIFIED.);
#66=B_SPLINE_CURVE_WITH_KNOTS('',3,(#3730,#3731,#3732,#3733,#3734,#3735,
#3736,#3737,#3738,#3739,#3740,#3741,#3742,#3743,#3744,#3745,#3746,#3747,
#3748,#3749,#3750,#3751,#3752,#3753,#3754,#3755,#3756,#3757,#3758,#3759,
#3760,#3761,#3762,#3763,#3764,#3765,#3766,#3767,#3768,#3769,#3770,#3771,
#3772,#3773,#3774,#3775,#3776,#3777,#3778,#3779,#3780,#3781,#3782,#3783,
#3784,#3785,#3786,#3787,#3788,#3789,#3790,#3791,#3792,#3793,#3794,#3795,
#3796,#3797,#3798,#3799,#3800,#3801,#3802,#3803,#3804,#3805,#3806,#3807,
#3808,#3809,#3810,#3811,#3812,#3813,#3814,#3815,#3816,#3817,#3818,#3819,
#3820,#3821,#3822,#3823,#3824,#3825,#3826,#3827,#3828,#3829,#3830,#3831,
#3832,#3833,#3834,#3835,#3836,#3837,#3838,#3839,#3840,#3841,#3842,#3843,
#3844,#3845,#3846,#3847,#3848,#3849,#3850,#3851,#3852,#3853,#3854,#3855,
#3856,#3857,#3858,#3859,#3860,#3861,#3862,#3863,#3864,#3865,#3866,#3867,
#3868,#3869,#3870,#3871,#3872,#3873,#3874,#3875,#3876,#3877,#3878,#3879,
#3880,#3881,#3882,#3883,#3884,#3885,#3886,#3887,#3888,#3889,#3890,#3891,
#3892,#3893,#3894,#3895,#3896,#3897,#3898,#3899,#3900,#3901,#3902,#3903,
#3904,#3905,#3906,#3907,#3908,#3909,#3910,#3911,#3912,#3913,#3914,#3915,
#3916,#3917,#3918,#3919,#3920,#3921,#3922,#3923,#3924,#3925),
 .UNSPECIFIED.,.F.,.F.,(4,2,2,2,2,2,2,2,2,2,2,2,2,2,2,2,2,2,2,2,2,2,2,2,
2,2,2,2,2,2,2,2,2,2,2,2,2,2,2,2,2,2,2,2,2,2,2,2,2,2,2,2,2,2,2,2,2,2,2,2,
2,2,2,2,2,2,2,2,2,2,2,2,2,2,2,2,2,2,2,2,2,2,2,2,2,2,2,2,2,2,2,2,2,2,2,2,
2,4),(-0.939600795071122,-0.932717148076296,-0.917632823774098,-0.9124005620682,
-0.908723319768595,-0.905379625484532,-0.899942432619131,-0.883717300430899,
-0.860937298427964,-0.847041736435776,-0.843517470395148,-0.841354761086481,
-0.839214912310399,-0.835798343305456,-0.822668703892458,-0.80575122815367,
-0.783436435022837,-0.777665319611758,-0.773886343430266,-0.770200819731045,
-0.764922551296239,-0.749376473166826,-0.721630035673222,-0.711176169236045,
-0.70789057995898,-0.705986402194631,-0.703851850256852,-0.700460890191082,
-0.687713974493037,-0.655791590508192,-0.645358358723685,-0.640767424507792,
-0.637175608797507,-0.633173640104625,-0.626292979332825,-0.617689148495527,
-0.596017374181675,-0.57803188698761,-0.573559118290177,-0.5711714763914,
-0.56934276614162,-0.566666047165555,-0.560449441082152,-0.525430769435245,
-0.511429584698833,-0.506199184352612,-0.502558836983457,-0.498776154320935,
-0.492985828748129,-0.468822278209715,-0.441775527532032,-0.437737050858496,
-0.435465320637159,-0.433396271425122,-0.430343182663081,-0.421364327021702,
-0.404369052008774,-0.379111419379661,-0.372364948337714,-0.368389832518859,
-0.364791513619253,-0.360069520952884,-0.349103523026432,-0.332151101588875,
-0.306687660057606,-0.302520813698895,-0.300198277096951,-0.298148246382424,
-0.295212728180463,-0.287207763946105,-0.273264386051648,-0.243145515932078,
-0.236697957531038,-0.232783084112019,-0.229166675364196,-0.224310979526816,
-0.212410122899578,-0.192924298824382,-0.171802139490986,-0.167329524256459,
-0.164941787808227,-0.163112898266531,-0.160435775156034,-0.154217572548377,
-0.11919175918273,-0.105194031282819,-0.0999635744661058,-0.0963229798264828,
-0.0925398662353551,-0.0921654860774136,-0.0918035472410569,-0.0914351641230606,
-0.0910427653025588,-0.0906068878656257,-0.0901031203839437,-0.08949837617733,
-0.0793554662889542,-0.0788478650889102),.UNSPECIFIED.);
#67=B_SPLINE_CURVE_WITH_KNOTS('',3,(#3930,#3931,#3932,#3933,#3934,#3935,
#3936,#3937,#3938,#3939,#3940,#3941,#3942,#3943,#3944,#3945,#3946,#3947,
#3948,#3949,#3950,#3951,#3952,#3953,#3954,#3955,#3956,#3957,#3958,#3959,
#3960,#3961,#3962,#3963,#3964,#3965,#3966,#3967,#3968,#3969,#3970,#3971,
#3972,#3973,#3974,#3975,#3976,#3977,#3978,#3979,#3980,#3981,#3982,#3983,
#3984,#3985,#3986,#3987,#3988,#3989,#3990,#3991,#3992,#3993,#3994,#3995,
#3996,#3997,#3998,#3999,#4000,#4001,#4002,#4003,#4004,#4005,#4006,#4007,
#4008,#4009,#4010,#4011,#4012,#4013,#4014,#4015,#4016,#4017,#4018,#4019,
#4020,#4021,#4022,#4023,#4024,#4025,#4026,#4027,#4028,#4029,#4030,#4031,
#4032,#4033,#4034,#4035,#4036,#4037,#4038,#4039,#4040,#4041,#4042,#4043,
#4044,#4045,#4046,#4047,#4048,#4049,#4050,#4051,#4052,#4053,#4054,#4055,
#4056,#4057,#4058,#4059,#4060,#4061,#4062,#4063,#4064,#4065,#4066,#4067,
#4068,#4069,#4070,#4071,#4072,#4073,#4074,#4075,#4076,#4077,#4078,#4079,
#4080,#4081,#4082,#4083,#4084,#4085,#4086,#4087,#4088,#4089,#4090,#4091,
#4092,#4093,#4094,#4095,#4096,#4097,#4098,#4099,#4100,#4101,#4102,#4103,
#4104,#4105,#4106,#4107,#4108,#4109),.UNSPECIFIED.,.F.,.F.,(4,2,2,2,2,2,
2,2,2,2,2,2,2,2,2,2,2,2,2,2,2,2,2,2,2,2,2,2,2,2,2,2,2,2,2,2,2,2,2,2,2,2,
2,2,2,2,2,2,2,2,2,2,2,2,2,2,2,2,2,2,2,2,2,2,2,2,2,2,2,2,2,2,2,2,2,2,2,2,
2,2,2,2,2,2,2,2,2,2,2,4),(-1.64346459097191,-1.64299413827663,-1.60796975239201,
-1.6017559312754,-1.59907926671871,-1.5972502157541,-1.59486139517667,-1.59038465729976,
-1.56963813329225,-1.54992778993481,-1.53795045785992,-1.53308401710661,
-1.5294655530535,-1.52555400213521,-1.51912511836203,-1.48882360767624,
-1.47496353663432,-1.46698761973969,-1.46405548679376,-1.46200570953533,
-1.45968076959513,-1.45550398171545,-1.4252496372731,-1.40838548913298,
-1.40056168432393,-1.39637401719785,-1.39280457146821,-1.38841267239701,
-1.38148422401653,-1.3504592528106,-1.3385868028233,-1.33134573927208,-1.32851313448038,
-1.32647704048686,-1.32410000184642,-1.31967922697425,-1.29884880166951,
-1.27913162015462,-1.26715197464246,-1.26228522492473,-1.25866672120616,
-1.25475530651898,-1.24832707393271,-1.21802031498721,-1.20416306979233,
-1.19618814522604,-1.19325614366897,-1.1912063888698,-1.18888139248743,
-1.1847043319608,-1.15938494526366,-1.142376348639,-1.13138780338708,-1.12666202358827,
-1.12306261093225,-1.11908800218368,-1.11234672668275,-1.08657737364282,
-1.06992745641147,-1.06105017813285,-1.05800822450704,-1.05594078084827,
-1.05366381075885,-1.04960170177527,-1.02277818054436,-0.998474338397782,
-0.992680506752823,-0.988896508027428,-0.985255508738456,-0.980025222524119,
-0.966039063831574,-0.9309824122132,-0.924760376413454,-0.922082302038895,
-0.920253017744464,-0.917864948848926,-0.913392116657112,-0.89399184135791,
-0.874466378027543,-0.861324738321179,-0.856307941661326,-0.852666281657645,
-0.848810171301246,-0.842656515975083,-0.817047434013356,-0.792599030371879,
-0.788367002157873,-0.786030038314498,-0.783983588999409,-0.782696160082662),
 .UNSPECIFIED.);
#68=B_SPLINE_CURVE_WITH_KNOTS('',3,(#4111,#4112,#4113,#4114,#4115,#4116,
#4117,#4118,#4119,#4120,#4121,#4122,#4123,#4124,#4125,#4126,#4127,#4128,
#4129,#4130),.UNSPECIFIED.,.F.,.F.,(4,2,2,2,2,2,2,2,2,4),(-0.0788478650889102,
-0.0642475044479353,-0.0404188851012244,-0.0332561931473402,-0.0303676396375803,
-0.0283245362340553,-0.0259788937490618,-0.0234388254342997,-0.0172068433153215,
-0.000387300569270395),.UNSPECIFIED.);
#69=B_SPLINE_CURVE_WITH_KNOTS('',3,(#4131,#4132,#4133,#4134,#4135,#4136,
#4137,#4138,#4139,#4140,#4141,#4142,#4143,#4144,#4145,#4146,#4147,#4148,
#4149,#4150,#4151,#4152,#4153,#4154,#4155,#4156,#4157,#4158,#4159,#4160,
#4161,#4162,#4163,#4164,#4165,#4166,#4167,#4168,#4169,#4170,#4171,#4172,
#4173,#4174,#4175,#4176,#4177,#4178,#4179,#4180,#4181,#4182,#4183,#4184,
#4185,#4186,#4187,#4188,#4189,#4190,#4191,#4192,#4193,#4194,#4195,#4196,
#4197,#4198,#4199,#4200,#4201,#4202,#4203,#4204,#4205,#4206,#4207,#4208,
#4209,#4210,#4211,#4212,#4213,#4214,#4215,#4216,#4217,#4218,#4219,#4220,
#4221,#4222,#4223,#4224,#4225,#4226,#4227,#4228,#4229,#4230,#4231,#4232,
#4233,#4234,#4235,#4236,#4237,#4238,#4239,#4240,#4241,#4242,#4243,#4244,
#4245,#4246,#4247,#4248,#4249,#4250,#4251,#4252,#4253,#4254,#4255,#4256,
#4257,#4258,#4259,#4260,#4261,#4262,#4263,#4264,#4265,#4266,#4267,#4268,
#4269,#4270,#4271,#4272,#4273,#4274,#4275,#4276,#4277,#4278,#4279,#4280,
#4281,#4282,#4283,#4284,#4285,#4286,#4287,#4288,#4289,#4290),
 .UNSPECIFIED.,.F.,.F.,(4,2,2,2,2,2,2,2,2,2,2,2,2,2,2,2,2,2,2,2,2,2,2,2,
2,2,2,2,2,2,2,2,2,2,2,2,2,2,2,2,2,2,2,2,2,2,2,2,2,2,2,2,2,2,2,2,2,2,2,2,
2,2,2,2,2,2,2,2,2,2,2,2,2,2,2,2,2,2,2,4),(-1.72212022081959,-1.69533255126009,
-1.69016620326192,-1.68548487803012,-1.68189175424043,-1.67789649965908,
-1.67104880052373,-1.64319535086452,-1.62817535772164,-1.61980786069624,
-1.61682697356166,-1.61477011898971,-1.61246876126964,-1.608287201836,-1.58276749554589,
-1.56583942628212,-1.55488319703798,-1.55016308540602,-1.54656530829544,
-1.54258989694887,-1.53584074254029,-1.51074305238622,-1.49361456735207,
-1.48459693358426,-1.48153955145949,-1.47946991782762,-1.47720016742003,
-1.47317058363322,-1.44607880187779,-1.4219757593487,-1.41618827508326,
-1.41240633530046,-1.40876588353763,-1.40353390814182,-1.38951623832309,
-1.35448975970563,-1.34827376895779,-1.34559715869928,-1.34376851903516,
-1.34138088223878,-1.33690805107266,-1.31755743222477,-1.29687415221088,
-1.28457549796112,-1.2796667260237,-1.27604277973669,-1.27214958370109,
-1.26580819035222,-1.23481396078216,-1.22131195958812,-1.21346267796392,
-1.21054746122841,-1.20850060609653,-1.20616853471792,-1.20195704402135,
-1.17711230455999,-1.15983401972054,-1.14874058829289,-1.14399999259999,
-1.14039947759935,-1.1364337461265,-1.1297333389673,-1.10254495760731,-1.08022989891291,
-1.0762296836793,-1.07396592620081,-1.07191704560627,-1.06886284387474,
-1.06054663348016,-1.03762421930456,-1.01561681822763,-1.00990048309864,
-1.00613206715272,-1.00248089192403,-0.997190584484555,-0.982741672931519,
-0.954828205269458,-0.94346779079941,-0.940181863111125,-0.939838537595481),
 .UNSPECIFIED.);
#70=B_SPLINE_CURVE_WITH_KNOTS('',3,(#4296,#4297,#4298,#4299,#4300,#4301,
#4302,#4303,#4304,#4305,#4306,#4307,#4308,#4309,#4310,#4311,#4312,#4313,
#4314,#4315,#4316,#4317,#4318,#4319,#4320,#4321,#4322,#4323,#4324,#4325,
#4326,#4327,#4328,#4329,#4330,#4331,#4332,#4333,#4334,#4335,#4336,#4337,
#4338,#4339,#4340,#4341,#4342,#4343,#4344,#4345,#4346,#4347,#4348,#4349,
#4350,#4351,#4352,#4353,#4354,#4355,#4356,#4357,#4358,#4359,#4360,#4361,
#4362,#4363,#4364,#4365,#4366,#4367,#4368,#4369,#4370,#4371,#4372,#4373,
#4374,#4375,#4376,#4377,#4378,#4379,#4380,#4381,#4382,#4383,#4384,#4385,
#4386,#4387,#4388,#4389,#4390,#4391,#4392,#4393,#4394,#4395,#4396,#4397,
#4398,#4399,#4400,#4401,#4402,#4403,#4404,#4405,#4406,#4407,#4408,#4409,
#4410,#4411,#4412,#4413,#4414,#4415,#4416,#4417,#4418,#4419,#4420,#4421,
#4422,#4423,#4424,#4425,#4426,#4427,#4428,#4429,#4430,#4431,#4432,#4433,
#4434,#4435,#4436,#4437,#4438,#4439,#4440,#4441,#4442,#4443,#4444,#4445,
#4446,#4447,#4448,#4449,#4450,#4451,#4452,#4453,#4454,#4455,#4456,#4457,
#4458,#4459,#4460,#4461),.UNSPECIFIED.,.F.,.F.,(4,2,2,2,2,2,2,2,2,2,2,2,
2,2,2,2,2,2,2,2,2,2,2,2,2,2,2,2,2,2,2,2,2,2,2,2,2,2,2,2,2,2,2,2,2,2,2,2,
2,2,2,2,2,2,2,2,2,2,2,2,2,2,2,2,2,2,2,2,2,2,2,2,2,2,2,2,2,2,2,2,2,2,4),
(-0.782502334421087,-0.767045137430122,-0.760820555065709,-0.756950338592601,
-0.753315532356511,-0.748340657637774,-0.735536528532295,-0.7146968730885,
-0.696198018516441,-0.691690477241836,-0.689295216228231,-0.687467210754608,
-0.684800027855247,-0.678644291391059,-0.639314047563905,-0.628542905584255,
-0.624194064720761,-0.620565714899577,-0.616762507239646,-0.610871077341131,
-0.584435900353066,-0.560325930300542,-0.556076684174118,-0.553736228853726,
-0.551691167046597,-0.548790976551945,-0.541057453264677,-0.527878239987123,
-0.496281099015622,-0.490024303065802,-0.486147684762659,-0.482515864686925,
-0.477559436979493,-0.464899611680007,-0.443058784216286,-0.425296645812249,
-0.420834926944211,-0.418449329304707,-0.416619786211475,-0.413938572024984,
-0.407696069476743,-0.372570046453006,-0.358693356814788,-0.353473085588776,
-0.349833950363349,-0.346047584087344,-0.340241238759429,-0.315445020904246,
-0.289242090673591,-0.285104823812511,-0.282812264812267,-0.280751252339647,
-0.27774749274177,-0.269194581030825,-0.253599217452694,-0.226310490821413,
-0.219616565852772,-0.215651556287467,-0.212049716427345,-0.207304402611245,
-0.196184105704066,-0.178836600102776,-0.154079317473949,-0.149861090993263,
-0.147527220035567,-0.145480106097394,-0.142566312897634,-0.134730784227824,
-0.121268670610156,-0.0902322400924257,-0.0838995623626038,-0.0800074554591401,
-0.076381670872289,-0.0714658787049653,-0.0591209858206712,-0.0337276219199564,
-0.0175107458707944,-0.0138931708560644,-0.0117101342163253,-0.0098247471181441,
-0.00768948435977741,-0.00452472033345642,-0.000387015215521824),
 .UNSPECIFIED.);
#71=B_SPLINE_CURVE_WITH_KNOTS('',3,(#4462,#4463,#4464,#4465,#4466,#4467,
#4468,#4469,#4470,#4471,#4472,#4473,#4474,#4475,#4476,#4477),
 .UNSPECIFIED.,.F.,.F.,(4,2,2,2,2,2,2,4),(-1.72208794112375,-1.69961702131751,
-1.67546164729257,-1.66967193793774,-1.66588887582809,-1.66224752994355,
-1.65701451805733,-1.64346459097191),.UNSPECIFIED.);
#72=B_SPLINE_CURVE_WITH_KNOTS('',3,(#4478,#4479,#4480,#4481,#4482,#4483,
#4484,#4485,#4486,#4487,#4488,#4489,#4490,#4491,#4492,#4493,#4494,#4495,
#4496,#4497,#4498,#4499,#4500,#4501,#4502,#4503,#4504,#4505,#4506,#4507,
#4508,#4509,#4510,#4511,#4512,#4513,#4514,#4515,#4516,#4517,#4518,#4519,
#4520,#4521,#4522,#4523,#4524,#4525,#4526,#4527,#4528,#4529,#4530,#4531,
#4532,#4533,#4534,#4535,#4536,#4537,#4538,#4539,#4540,#4541,#4542,#4543,
#4544,#4545,#4546,#4547,#4548,#4549,#4550,#4551,#4552,#4553,#4554,#4555,
#4556,#4557,#4558,#4559,#4560,#4561,#4562,#4563,#4564,#4565,#4566,#4567,
#4568,#4569,#4570,#4571,#4572,#4573,#4574,#4575,#4576,#4577,#4578,#4579,
#4580,#4581,#4582,#4583,#4584,#4585,#4586,#4587,#4588,#4589,#4590,#4591,
#4592,#4593,#4594,#4595,#4596,#4597,#4598,#4599,#4600,#4601,#4602,#4603,
#4604,#4605,#4606,#4607,#4608,#4609,#4610,#4611,#4612,#4613,#4614,#4615,
#4616,#4617,#4618,#4619,#4620,#4621,#4622,#4623,#4624,#4625,#4626,#4627,
#4628,#4629,#4630,#4631,#4632,#4633,#4634,#4635,#4636,#4637,#4638,#4639,
#4640,#4641,#4642,#4643,#4644,#4645,#4646,#4647,#4648,#4649,#4650,#4651,
#4652,#4653,#4654,#4655,#4656,#4657),.UNSPECIFIED.,.F.,.F.,(4,2,2,2,2,2,
2,2,2,2,2,2,2,2,2,2,2,2,2,2,2,2,2,2,2,2,2,2,2,2,2,2,2,2,2,2,2,2,2,2,2,2,
2,2,2,2,2,2,2,2,2,2,2,2,2,2,2,2,2,2,2,2,2,2,2,2,2,2,2,2,2,2,2,2,2,2,2,2,
2,2,2,2,2,2,2,2,2,2,2,4),(-0.939838537595481,-0.938068797775664,-0.936145440061214,
-0.932756964776017,-0.92121159401672,-0.893145310333023,-0.878928004304586,
-0.873786974217987,-0.870125352159042,-0.866763503213755,-0.861221197153815,
-0.842434949502465,-0.827724190822388,-0.810285819065485,-0.805837941971229,
-0.803455451934922,-0.801420979433844,-0.7985992975301,-0.791432461321423,
-0.779749286419483,-0.749483422745094,-0.741276929095984,-0.736967781883236,
-0.733401271993392,-0.729141678050981,-0.720934899560516,-0.709972122574217,
-0.69341145547469,-0.674979783703478,-0.670477739758828,-0.6680838892394,
-0.666256103659589,-0.663588218243026,-0.657426430809991,-0.618074466313829,
-0.607320212510232,-0.60297435246546,-0.599347192523239,-0.595543931751392,
-0.589649763658981,-0.563038803090738,-0.539140753286892,-0.534870759234907,
-0.532526113872392,-0.530482759766023,-0.527592431394132,-0.519930340622053,
-0.506946582747292,-0.474944196487876,-0.468743476837958,-0.464878666674533,
-0.461242709787195,-0.456256322976876,-0.443355305630278,-0.422210296904462,
-0.404094785254174,-0.399614521128156,-0.397225295663127,-0.395396838270499,
-0.392722422317909,-0.386520084878706,-0.346968952183938,-0.336339042098344,
-0.331616227157014,-0.328007256916538,-0.324072138519676,-0.31752248052578,
-0.297371999190207,-0.274791687277466,-0.266029135469896,-0.262918384678814,
-0.260859806833145,-0.258617255382973,-0.254717078326282,-0.233608482817605,
-0.204869286252108,-0.198278878746309,-0.194335669425123,-0.190729386192128,
-0.185942115507579,-0.174525341677054,-0.156391882314086,-0.133075844426758,
-0.128718098421515,-0.126354903223532,-0.124316577615172,-0.121461996238531,
-0.11405990954294,-0.101769993493656,-0.079052177473784),.UNSPECIFIED.);
#73=B_SPLINE_CURVE_WITH_KNOTS('',3,(#4662,#4663,#4664,#4665,#4666,#4667,
#4668,#4669,#4670,#4671,#4672,#4673,#4674,#4675,#4676,#4677,#4678,#4679,
#4680,#4681,#4682,#4683,#4684,#4685,#4686,#4687,#4688,#4689,#4690,#4691,
#4692,#4693,#4694,#4695,#4696,#4697,#4698,#4699,#4700,#4701,#4702,#4703,
#4704,#4705,#4706,#4707,#4708,#4709,#4710,#4711,#4712,#4713,#4714,#4715,
#4716,#4717,#4718,#4719,#4720,#4721,#4722,#4723,#4724,#4725,#4726,#4727,
#4728,#4729,#4730,#4731,#4732,#4733,#4734,#4735,#4736,#4737,#4738,#4739,
#4740,#4741,#4742,#4743,#4744,#4745,#4746,#4747,#4748,#4749,#4750,#4751,
#4752,#4753,#4754,#4755,#4756,#4757,#4758,#4759,#4760,#4761,#4762,#4763,
#4764,#4765,#4766,#4767,#4768,#4769,#4770,#4771,#4772,#4773,#4774,#4775,
#4776,#4777,#4778,#4779,#4780,#4781,#4782,#4783,#4784,#4785,#4786,#4787,
#4788,#4789,#4790,#4791,#4792,#4793,#4794,#4795,#4796,#4797,#4798,#4799,
#4800,#4801,#4802,#4803,#4804,#4805,#4806,#4807,#4808,#4809,#4810,#4811,
#4812,#4813,#4814,#4815,#4816,#4817,#4818,#4819,#4820,#4821,#4822,#4823,
#4824,#4825,#4826,#4827,#4828,#4829,#4830,#4831,#4832,#4833,#4834,#4835,
#4836,#4837,#4838,#4839,#4840,#4841,#4842,#4843,#4844,#4845),
 .UNSPECIFIED.,.F.,.F.,(4,2,2,2,2,2,2,2,2,2,2,2,2,2,2,2,2,2,2,2,2,2,2,2,
2,2,2,2,2,2,2,2,2,2,2,2,2,2,2,2,2,2,2,2,2,2,2,2,2,2,2,2,2,2,2,2,2,2,2,2,
2,2,2,2,2,2,2,2,2,2,2,2,2,2,2,2,2,2,2,2,2,2,2,2,2,2,2,2,2,2,2,4),(-1.64297773443279,
-1.64004297846864,-1.63736524041581,-1.63553677967994,-1.63315064508125,
-1.62868346378423,-1.61077294092021,-1.58951056936148,-1.57657617060184,
-1.57158667665708,-1.56795085702201,-1.56408830249779,-1.55789591873041,
-1.52584075523492,-1.51288115910944,-1.50522919089457,-1.50234061161371,
-1.50029788278035,-1.49795303213325,-1.4936806392777,-1.46985579832729,
-1.45199849669385,-1.44068579653118,-1.43591394403918,-1.43230994527066,
-1.42836010309057,-1.42173585057647,-1.39339076853442,-1.37196237222845,
-1.36805141050512,-1.36580669791819,-1.36374935765044,-1.36064508749538,
-1.35193258783187,-1.32934059477822,-1.30919179992477,-1.30264298564033,
-1.29870819515655,-1.29509932434392,-1.29037628677091,-1.27992407545554,
-1.24748833893756,-1.23551372973242,-1.23217916097273,-1.23005644605728,
-1.2278739478477,-1.22425667230072,-1.20814517415559,-1.18397167511406,
-1.17065875800202,-1.16562247331685,-1.16197872269448,-1.15813114870345,
-1.15201503415923,-1.11941795249295,-1.10671426468329,-1.10150099922408,
-1.0974516555762,-1.0951777226073,-1.09313335842651,-1.09010535364877,-1.08198499486996,
-1.05891403633355,-1.04415768158023,-1.03717629397825,-1.03129407456293,
-1.02749306514734,-1.02386417573296,-1.01951146533365,-1.00871276681361,
-0.969394484886577,-0.963242986690139,-0.960576607405278,-0.95874884174587,
-0.956353365951283,-0.951844283119531,-0.933327549125823,-0.916567056098586,
-0.900565618543884,-0.8952442532579,-0.891550456425138,-0.887780882267833,
-0.882060112836508,-0.86097354370312,-0.831179280780422,-0.8269165479703,
-0.824573143044055,-0.822528794713476,-0.819634103208903,-0.811942321610842,
-0.79887808948178,-0.782502334421087),.UNSPECIFIED.);
#74=B_SPLINE_CURVE_WITH_KNOTS('',3,(#4847,#4848,#4849,#4850,#4851,#4852,
#4853,#4854,#4855,#4856,#4857,#4858,#4859,#4860,#4861,#4862),
 .UNSPECIFIED.,.F.,.F.,(4,2,2,2,2,2,2,4),(-0.079052177473784,-0.0689809976460656,
-0.0626536956613715,-0.0587636537041857,-0.0551390412965591,-0.050223731628864,
-0.0378738902713093,-0.000387745880559849),.UNSPECIFIED.);
#75=B_SPLINE_CURVE_WITH_KNOTS('',3,(#4863,#4864,#4865,#4866,#4867,#4868,
#4869,#4870,#4871,#4872,#4873,#4874,#4875,#4876,#4877,#4878,#4879,#4880,
#4881,#4882,#4883,#4884,#4885,#4886,#4887,#4888,#4889,#4890,#4891,#4892,
#4893,#4894,#4895,#4896,#4897,#4898,#4899,#4900,#4901,#4902,#4903,#4904,
#4905,#4906,#4907,#4908,#4909,#4910,#4911,#4912,#4913,#4914,#4915,#4916,
#4917,#4918,#4919,#4920,#4921,#4922,#4923,#4924,#4925,#4926,#4927,#4928,
#4929,#4930,#4931,#4932,#4933,#4934,#4935,#4936,#4937,#4938,#4939,#4940,
#4941,#4942,#4943,#4944,#4945,#4946,#4947,#4948,#4949,#4950,#4951,#4952,
#4953,#4954,#4955,#4956,#4957,#4958,#4959,#4960,#4961,#4962,#4963,#4964,
#4965,#4966,#4967,#4968,#4969,#4970,#4971,#4972,#4973,#4974,#4975,#4976,
#4977,#4978,#4979,#4980,#4981,#4982,#4983,#4984,#4985,#4986,#4987,#4988,
#4989,#4990,#4991,#4992,#4993,#4994,#4995,#4996,#4997,#4998,#4999,#5000,
#5001,#5002,#5003,#5004,#5005,#5006,#5007,#5008,#5009,#5010,#5011,#5012,
#5013,#5014,#5015,#5016,#5017,#5018,#5019,#5020,#5021,#5022,#5023,#5024,
#5025,#5026,#5027,#5028,#5029,#5030,#5031,#5032),.UNSPECIFIED.,.F.,.F.,
(4,2,2,2,2,2,2,2,2,2,2,2,2,2,2,2,2,2,2,2,2,2,2,2,2,2,2,2,2,2,2,2,2,2,2,
2,2,2,2,2,2,2,2,2,2,2,2,2,2,2,2,2,2,2,2,2,2,2,2,2,2,2,2,2,2,2,2,2,2,2,2,
2,2,2,2,2,2,2,2,2,2,2,2,2,4),(-1.72202346959793,-1.71870018917094,-1.71591322745448,
-1.7137717851489,-1.71189119546824,-1.70971791514103,-1.70614322261802,
-1.69104856008632,-1.66138713746971,-1.65436780756703,-1.64846163132073,
-1.64465642502085,-1.64103140026988,-1.63669289250378,-1.62598523221138,
-1.58656459426751,-1.58039020467346,-1.57772042206146,-1.57589261844911,
-1.57350052300544,-1.56900615173947,-1.55067513426042,-1.53420116499451,
-1.52315305398727,-1.51490055503334,-1.5106327586612,-1.5070666719527,-1.50276688016783,
-1.49460698831665,-1.46426952076207,-1.45256578852821,-1.44539135107234,
-1.44256868709891,-1.44053426948862,-1.43815268817646,-1.433708588999,-1.41274055928829,
-1.39314353539268,-1.38120527695429,-1.37634492977801,-1.37272814275904,
-1.36881576233835,-1.36237934197206,-1.33214526514168,-1.31824831572467,
-1.31025989639583,-1.30732661631416,-1.30527710798275,-1.30295384133811,
-1.29878306781289,-1.27339646693931,-1.25642332096652,-1.24544916521034,
-1.24072627291106,-1.23712804079784,-1.23315377705416,-1.22641079352668,
-1.20080262310378,-1.18403711853035,-1.17512584778449,-1.17208047826183,
-1.17001286668314,-1.16773829430545,-1.16368587832871,-1.13678362319376,
-1.11253716635762,-1.10674568648551,-1.10296285987455,-1.09932277953469,
-1.09409352460756,-1.08010956202237,-1.04505169166033,-1.03882770328252,
-1.03614973459047,-1.03432088144703,-1.0319339998225,-1.02746502477973,
-1.00785201787439,-0.987346036116553,-0.975104496453811,-0.970203164133492,
-0.966580221846493,-0.962683928260761,-0.956327698005292,-0.939927914600591),
 .UNSPECIFIED.);
#76=B_SPLINE_CURVE_WITH_KNOTS('',3,(#5038,#5039,#5040,#5041,#5042,#5043,
#5044,#5045,#5046,#5047,#5048,#5049,#5050,#5051,#5052,#5053,#5054,#5055,
#5056,#5057,#5058,#5059,#5060,#5061,#5062,#5063,#5064,#5065,#5066,#5067,
#5068,#5069,#5070,#5071,#5072,#5073,#5074,#5075,#5076,#5077,#5078,#5079,
#5080,#5081,#5082,#5083,#5084,#5085,#5086,#5087,#5088,#5089,#5090,#5091,
#5092,#5093,#5094,#5095,#5096,#5097,#5098,#5099,#5100,#5101,#5102,#5103,
#5104,#5105,#5106,#5107,#5108,#5109,#5110,#5111,#5112,#5113,#5114,#5115,
#5116,#5117,#5118,#5119,#5120,#5121,#5122,#5123,#5124,#5125,#5126,#5127,
#5128,#5129,#5130,#5131,#5132,#5133,#5134,#5135,#5136,#5137,#5138,#5139,
#5140,#5141,#5142,#5143,#5144,#5145,#5146,#5147,#5148,#5149,#5150,#5151,
#5152,#5153,#5154,#5155,#5156,#5157,#5158,#5159,#5160,#5161,#5162,#5163,
#5164,#5165,#5166,#5167,#5168,#5169,#5170,#5171,#5172,#5173,#5174,#5175,
#5176,#5177,#5178,#5179,#5180,#5181,#5182,#5183,#5184,#5185,#5186,#5187,
#5188,#5189,#5190,#5191,#5192,#5193,#5194,#5195,#5196,#5197,#5198,#5199),
 .UNSPECIFIED.,.F.,.F.,(4,2,2,2,2,2,2,2,2,2,2,2,2,2,2,2,2,2,2,2,2,2,2,2,
2,2,2,2,2,2,2,2,2,2,2,2,2,2,2,2,2,2,2,2,2,2,2,2,2,2,2,2,2,2,2,2,2,2,2,2,
2,2,2,2,2,2,2,2,2,2,2,2,2,2,2,2,2,2,2,2,4),(-0.782686723559536,-0.776829908385411,
-0.759694909346261,-0.734557343110431,-0.730361867686715,-0.728032581521128,
-0.725983481676664,-0.723058616281106,-0.715141620403665,-0.701451820327158,
-0.670845737253636,-0.664455565957333,-0.660551250214299,-0.656928984029553,
-0.652041174517008,-0.639912390951821,-0.619755546974085,-0.59969774299674,
-0.595168709446075,-0.59276859020319,-0.590940797163087,-0.588279083002747,
-0.582159300687959,-0.542994182076116,-0.532060526505425,-0.527686745055492,
-0.524051907850687,-0.520256669090037,-0.514408754673189,-0.507481153357872,
-0.492921967070446,-0.464062707929007,-0.459637131773207,-0.457258779161931,
-0.455222391313416,-0.452390588694543,-0.445157569901286,-0.433307848590126,
-0.402366183445107,-0.395384280391682,-0.390976944941689,-0.387406028922544,
-0.38322918423663,-0.375465214483068,-0.36010030753842,-0.335487379845948,
-0.326223078674156,-0.323051662153072,-0.320981173404627,-0.318757117138205,
-0.314947944026571,-0.310141239047756,-0.299043161632813,-0.264788713760983,
-0.258261368828698,-0.254329590727207,-0.250717305906561,-0.245897130031362,
-0.234258739925162,-0.215521604929568,-0.193128150007976,-0.188753124981894,
-0.186385553465706,-0.184346916354634,-0.181496453706521,-0.174130198356016,
-0.161936407667949,-0.129559513557705,-0.122930531688521,-0.11897822899014,
-0.115372169487496,-0.110597877453516,-0.0992818286751014,-0.0814224240349977,
-0.0575323651140709,-0.0532602224953532,-0.0509145690988358,-0.0488703999603477,
-0.0459788792694939,-0.0383129958008827,-0.000387729151872138),
 .UNSPECIFIED.);
#77=B_SPLINE_CURVE_WITH_KNOTS('',3,(#5200,#5201,#5202,#5203,#5204,#5205,
#5206,#5207,#5208,#5209,#5210,#5211,#5212,#5213,#5214,#5215,#5216,#5217,
#5218,#5219),.UNSPECIFIED.,.F.,.F.,(4,2,2,2,2,2,2,2,2,4),(-1.7216012596671,
-1.71550655685447,-1.71067082519282,-1.70705039597375,-1.70367348907421,
-1.69990717799663,-1.69419743381424,-1.67243675688787,-1.64626826175847,
-1.64297773443279),.UNSPECIFIED.);
#78=B_SPLINE_CURVE_WITH_KNOTS('',3,(#5220,#5221,#5222,#5223,#5224,#5225,
#5226,#5227,#5228,#5229,#5230,#5231,#5232,#5233,#5234,#5235,#5236,#5237,
#5238,#5239,#5240,#5241,#5242,#5243,#5244,#5245,#5246,#5247,#5248,#5249,
#5250,#5251,#5252,#5253,#5254,#5255,#5256,#5257,#5258,#5259,#5260,#5261,
#5262,#5263,#5264,#5265,#5266,#5267,#5268,#5269,#5270,#5271,#5272,#5273,
#5274,#5275,#5276,#5277,#5278,#5279,#5280,#5281,#5282,#5283,#5284,#5285,
#5286,#5287,#5288,#5289,#5290,#5291,#5292,#5293,#5294,#5295,#5296,#5297,
#5298,#5299,#5300,#5301,#5302,#5303,#5304,#5305,#5306,#5307,#5308,#5309,
#5310,#5311,#5312,#5313,#5314,#5315,#5316,#5317,#5318,#5319,#5320,#5321,
#5322,#5323,#5324,#5325,#5326,#5327,#5328,#5329,#5330,#5331,#5332,#5333,
#5334,#5335,#5336,#5337,#5338,#5339,#5340,#5341,#5342,#5343,#5344,#5345,
#5346,#5347,#5348,#5349,#5350,#5351,#5352,#5353,#5354,#5355,#5356,#5357,
#5358,#5359,#5360,#5361,#5362,#5363,#5364,#5365,#5366,#5367,#5368,#5369,
#5370,#5371,#5372,#5373,#5374,#5375,#5376,#5377,#5378,#5379,#5380,#5381,
#5382,#5383,#5384,#5385,#5386,#5387,#5388,#5389,#5390,#5391,#5392,#5393,
#5394,#5395,#5396,#5397,#5398,#5399),.UNSPECIFIED.,.F.,.F.,(4,2,2,2,2,2,
2,2,2,2,2,2,2,2,2,2,2,2,2,2,2,2,2,2,2,2,2,2,2,2,2,2,2,2,2,2,2,2,2,2,2,2,
2,2,2,2,2,2,2,2,2,2,2,2,2,2,2,2,2,2,2,2,2,2,2,2,2,2,2,2,2,2,2,2,2,2,2,2,
2,2,2,2,2,2,2,2,2,2,2,4),(-0.939927914600591,-0.923554267701752,-0.911263480236345,
-0.906151124386267,-0.902160808727174,-0.899899068576791,-0.897849160525681,
-0.895284635018434,-0.888528660992351,-0.861444729901312,-0.841498237755948,
-0.835805365716651,-0.832041454714497,-0.828343759470433,-0.822999889948548,
-0.806753459006284,-0.790151906013408,-0.771714213525448,-0.767211576534864,
-0.764817540605371,-0.762989691557827,-0.760321816451003,-0.754160522112188,
-0.714810511893886,-0.704052537395685,-0.69970600330477,-0.69607857650783,
-0.69227534293082,-0.686381870447858,-0.659822843986647,-0.635855765468199,
-0.631593179933376,-0.629250061396491,-0.62720617584421,-0.624312555995763,
-0.616626522513446,-0.603577728127068,-0.571706183948792,-0.565486635879485,
-0.561617914336139,-0.55798347915703,-0.553007531340048,-0.540190887178216,
-0.519312299844477,-0.500856611132237,-0.496352703931226,-0.493958460860715,
-0.492130734998392,-0.489463410509781,-0.483305077279369,-0.443969649384891,
-0.433200361860738,-0.428852240868508,-0.425224551848086,-0.421422145459688,
-0.41553229912841,-0.389160708630153,-0.364969131690273,-0.360725430270745,
-0.358386419990707,-0.356341495739722,-0.353440089561388,-0.345695155792632,
-0.332484176260121,-0.300944076448628,-0.294679124014928,-0.290801335785631,
-0.28717102974285,-0.282220894810267,-0.269606293613773,-0.247915109770964,
-0.22995397359159,-0.225482475353296,-0.223095079153693,-0.221266294767036,
-0.218589120229558,-0.212369847080465,-0.177340680088108,-0.163350705858965,
-0.158121205009425,-0.154480976403562,-0.150697992740656,-0.144906326348576,
-0.120694903844777,-0.0937113529293291,-0.0896652440295716,-0.0873919005455655,
-0.0853235244697597,-0.0822744434035082,-0.0790377234486064),
 .UNSPECIFIED.);
#79=B_SPLINE_CURVE_WITH_KNOTS('',3,(#5404,#5405,#5406,#5407,#5408,#5409,
#5410,#5411,#5412,#5413,#5414,#5415,#5416,#5417,#5418,#5419,#5420,#5421,
#5422,#5423,#5424,#5425,#5426,#5427,#5428,#5429,#5430,#5431,#5432,#5433,
#5434,#5435,#5436,#5437,#5438,#5439,#5440,#5441,#5442,#5443,#5444,#5445,
#5446,#5447,#5448,#5449,#5450,#5451,#5452,#5453,#5454,#5455,#5456,#5457,
#5458,#5459,#5460,#5461,#5462,#5463,#5464,#5465,#5466,#5467,#5468,#5469,
#5470,#5471,#5472,#5473,#5474,#5475,#5476,#5477,#5478,#5479,#5480,#5481,
#5482,#5483,#5484,#5485,#5486,#5487,#5488,#5489,#5490,#5491,#5492,#5493,
#5494,#5495,#5496,#5497,#5498,#5499,#5500,#5501,#5502,#5503,#5504,#5505,
#5506,#5507,#5508,#5509,#5510,#5511,#5512,#5513,#5514,#5515,#5516,#5517,
#5518,#5519,#5520,#5521,#5522,#5523,#5524,#5525,#5526,#5527,#5528,#5529,
#5530,#5531,#5532,#5533,#5534,#5535,#5536,#5537,#5538,#5539,#5540,#5541,
#5542,#5543,#5544,#5545,#5546,#5547,#5548,#5549,#5550,#5551,#5552,#5553,
#5554,#5555,#5556,#5557,#5558,#5559,#5560,#5561,#5562,#5563,#5564,#5565,
#5566,#5567,#5568,#5569,#5570,#5571,#5572,#5573,#5574,#5575,#5576,#5577,
#5578,#5579,#5580,#5581,#5582,#5583,#5584,#5585),.UNSPECIFIED.,.F.,.F.,
(4,2,2,2,2,2,2,2,2,2,2,2,2,2,2,2,2,2,2,2,2,2,2,2,2,2,2,2,2,2,2,2,2,2,2,
2,2,2,2,2,2,2,2,2,2,2,2,2,2,2,2,2,2,2,2,2,2,2,2,2,2,2,2,2,2,2,2,2,2,2,2,
2,2,2,2,2,2,2,2,2,2,2,2,2,2,2,2,2,2,2,4),(-1.64347692384346,-1.62647809996023,
-1.61519114415661,-1.61042132461924,-1.60681599358851,-1.60286189606256,
-1.59622352561842,-1.56799895904397,-1.55296545702111,-1.54459279077102,
-1.54161057888925,-1.53955290587183,-1.53725064258264,-1.53306729168193,
-1.50730452913988,-1.48519766988736,-1.47777616399101,-1.47366614387183,
-1.47009017055522,-1.46559487452762,-1.45829221621878,-1.42776139810831,
-1.41601010631762,-1.40881638020244,-1.40599037167774,-1.40395495039513,
-1.40157378419175,-1.39713398687239,-1.37630457460847,-1.35660549186341,
-1.34463156987632,-1.33976533813434,-1.33614667502193,-1.33223457484849,
-1.32580399123308,-1.29550999255385,-1.28164359657382,-1.27366522418574,
-1.27073262439214,-1.26868265014921,-1.26635763912456,-1.2621810428845,
-1.23685037511258,-1.21984546503079,-1.20885802194901,-1.20413215610088,
-1.20053248952346,-1.1965574136866,-1.18981486861127,-1.16409070196488,
-1.1474060751908,-1.13851813470799,-1.13547479302475,-1.13340698664667,
-1.13113028681442,-1.12707002523676,-1.10022602928524,-1.07593398004563,
-1.07014003585567,-1.06635580272923,-1.06271446363032,-1.05748348543213,
-1.04349301673887,-1.00843634258165,-1.00221452490058,-0.999536351783928,
-0.997706933977108,-0.995318595178487,-0.990845031998848,-0.971471413028527,
-0.951982264612179,-0.938789164943159,-0.933765807222672,-0.930122869243032,
-0.926268514868687,-0.92012460735921,-0.887685197354395,-0.874893619944347,
-0.869658103041326,-0.865595303780987,-0.863317917160893,-0.861273638061288,
-0.858250270910351,-0.8495357104705,-0.833424756299311,-0.806900675158636,
-0.800175522456143,-0.796203645093578,-0.792602586738466,-0.787868619119288,
-0.782686723559536),.UNSPECIFIED.);
#80=B_SPLINE_CURVE_WITH_KNOTS('',3,(#5587,#5588,#5589,#5590,#5591,#5592,
#5593,#5594,#5595,#5596,#5597,#5598,#5599,#5600,#5601,#5602,#5603,#5604,
#5605,#5606),.UNSPECIFIED.,.F.,.F.,(4,2,2,2,2,2,2,2,2,4),(-0.0790377234486064,
-0.0733310779424561,-0.0519587194341138,-0.0310138573416728,-0.0242790937925843,
-0.0203062843425282,-0.0168350967339937,-0.0133427717109691,-0.00781598579281862,
-0.0003870511716117),.UNSPECIFIED.);
#81=B_SPLINE_CURVE_WITH_KNOTS('',3,(#5607,#5608,#5609,#5610,#5611,#5612,
#5613,#5614,#5615,#5616,#5617,#5618,#5619,#5620,#5621,#5622,#5623,#5624,
#5625,#5626,#5627,#5628,#5629,#5630,#5631,#5632,#5633,#5634,#5635,#5636,
#5637,#5638,#5639,#5640,#5641,#5642,#5643,#5644,#5645,#5646,#5647,#5648,
#5649,#5650,#5651,#5652,#5653,#5654,#5655,#5656,#5657,#5658,#5659,#5660,
#5661,#5662,#5663,#5664,#5665,#5666,#5667,#5668,#5669,#5670,#5671,#5672,
#5673,#5674,#5675,#5676,#5677,#5678,#5679,#5680,#5681,#5682,#5683,#5684,
#5685,#5686,#5687,#5688,#5689,#5690,#5691,#5692,#5693,#5694,#5695,#5696,
#5697,#5698,#5699,#5700,#5701,#5702,#5703,#5704,#5705,#5706,#5707,#5708,
#5709,#5710,#5711,#5712,#5713,#5714,#5715,#5716,#5717,#5718,#5719,#5720,
#5721,#5722,#5723,#5724,#5725,#5726,#5727,#5728,#5729,#5730,#5731,#5732,
#5733,#5734,#5735,#5736,#5737,#5738,#5739,#5740,#5741,#5742,#5743,#5744,
#5745,#5746,#5747,#5748,#5749,#5750,#5751,#5752,#5753,#5754,#5755,#5756,
#5757,#5758,#5759,#5760,#5761,#5762,#5763,#5764,#5765,#5766,#5767,#5768),
 .UNSPECIFIED.,.F.,.F.,(4,2,2,2,2,2,2,2,2,2,2,2,2,2,2,2,2,2,2,2,2,2,2,2,
2,2,2,2,2,2,2,2,2,2,2,2,2,2,2,2,2,2,2,2,2,2,2,2,2,2,2,2,2,2,2,2,2,2,2,2,
2,2,2,2,2,2,2,2,2,2,2,2,2,2,2,2,2,2,2,2,4),(-1.72190052015242,-1.7008417553696,
-1.67959684492697,-1.67569206404128,-1.6734487908009,-1.67139110028624,
-1.66828400795561,-1.65954762801523,-1.63696924262774,-1.62239240996895,
-1.6124236064941,-1.60785759134824,-1.60427728045063,-1.60021747719425,
-1.593234689959,-1.56143533771465,-1.54937567616379,-1.54206258327152,-1.53922055996786,
-1.53718403671187,-1.53481422723463,-1.53042470441813,-1.50743773593717,
-1.48914697124183,-1.47767246073601,-1.47287730510484,-1.46927016858056,
-1.46533092948403,-1.45875935533647,-1.42979099186425,-1.40901528198744,
-1.40502214366069,-1.40276013650602,-1.40071104751257,-1.39765395885015,
-1.38931286139406,-1.36641605531578,-1.35172163584231,-1.34475752822906,
-1.33888643933257,-1.33508796435709,-1.33145829623413,-1.32710082120996,
-1.31626833493528,-1.27698090133382,-1.27083455163844,-1.26816919426628,
-1.26634174274867,-1.26394622361528,-1.25943612937136,-1.2409066312412,
-1.22400969584118,-1.20812458662231,-1.20281426740824,-1.19912282053708,
-1.19579244388631,-1.19043602103518,-1.17513555137222,-1.14806746104473,
-1.13684265131668,-1.13356817698875,-1.13145744408986,-1.12925859429158,
-1.12556550075609,-1.10527641878139,-1.08422458841688,-1.07180817690105,
-1.06688369388516,-1.06325716571645,-1.05936953824415,-1.05305664542918,
-1.02184004167219,-1.00844868028128,-1.00063872648701,-0.997728541971604,
-0.995682297284709,-0.993347454769666,-0.989123585235036,-0.964517292391267,
-0.947095091498651,-0.939896813873088),.UNSPECIFIED.);
#82=B_SPLINE_CURVE_WITH_KNOTS('',3,(#5774,#5775,#5776,#5777,#5778,#5779,
#5780,#5781,#5782,#5783,#5784,#5785,#5786,#5787,#5788,#5789,#5790,#5791,
#5792,#5793,#5794,#5795,#5796,#5797,#5798,#5799,#5800,#5801,#5802,#5803,
#5804,#5805,#5806,#5807,#5808,#5809,#5810,#5811,#5812,#5813,#5814,#5815,
#5816,#5817,#5818,#5819,#5820,#5821,#5822,#5823,#5824,#5825,#5826,#5827,
#5828,#5829,#5830,#5831,#5832,#5833,#5834,#5835,#5836,#5837,#5838,#5839,
#5840,#5841,#5842,#5843,#5844,#5845,#5846,#5847,#5848,#5849,#5850,#5851,
#5852,#5853,#5854,#5855,#5856,#5857,#5858,#5859,#5860,#5861,#5862,#5863,
#5864,#5865,#5866,#5867,#5868,#5869,#5870,#5871,#5872,#5873,#5874,#5875,
#5876,#5877,#5878,#5879,#5880,#5881,#5882,#5883,#5884,#5885,#5886,#5887,
#5888,#5889,#5890,#5891,#5892,#5893,#5894,#5895,#5896,#5897,#5898,#5899,
#5900,#5901,#5902,#5903,#5904,#5905,#5906,#5907,#5908,#5909,#5910,#5911,
#5912,#5913,#5914,#5915,#5916,#5917,#5918,#5919,#5920,#5921,#5922,#5923,
#5924,#5925,#5926,#5927,#5928,#5929,#5930,#5931,#5932,#5933,#5934,#5935,
#5936,#5937,#5938,#5939,#5940,#5941,#5942,#5943),.UNSPECIFIED.,.F.,.F.,
(4,2,2,2,2,2,2,2,2,2,2,2,2,2,2,2,2,2,2,2,2,2,2,2,2,2,2,2,2,2,2,2,2,2,2,
2,2,2,2,2,2,2,2,2,2,2,2,2,2,2,2,2,2,2,2,2,2,2,2,2,2,2,2,2,2,2,2,2,2,2,2,
2,2,2,2,2,2,2,2,2,2,2,2,2,4),(-0.782599245859888,-0.771916842875543,-0.768391423183112,
-0.766228283301738,-0.764087894668306,-0.760670671928447,-0.747540096293486,
-0.730623483154982,-0.708310536159541,-0.702538578495944,-0.698758569476279,
-0.695071619029943,-0.689790445592084,-0.674224150558897,-0.647851420333512,
-0.636273406736027,-0.632881734529875,-0.630957404873542,-0.628844178174779,
-0.625559134319365,-0.614211710202638,-0.586364196575075,-0.57187831405912,
-0.566584986678905,-0.562932722225909,-0.559163930256809,-0.553448506717713,
-0.531494501426773,-0.508671845943224,-0.500210245250518,-0.497136751173071,
-0.49508424883467,-0.492826991589006,-0.488859202040587,-0.483785807980474,
-0.471650989715129,-0.439521106204485,-0.432714938328506,-0.42872740732765,
-0.42513134972042,-0.420431868479238,-0.409618826514158,-0.393050433566889,
-0.366862294429662,-0.362723062780961,-0.360430053398802,-0.358369095119043,
-0.355366090293615,-0.346820294776242,-0.331247934685562,-0.303921333544282,
-0.297228910757118,-0.293264060986159,-0.289661921055439,-0.284915551415741,
-0.2737891873953,-0.256426444227997,-0.231693102888949,-0.227473457318857,
-0.225139198332099,-0.223092057284232,-0.220178629888363,-0.212346522643491,
-0.198894354670003,-0.167835990360443,-0.161505766506546,-0.15761404881174,
-0.153987900294494,-0.149070474775887,-0.136714204326878,-0.115854771085359,
-0.0952920913959404,-0.0915829562950598,-0.0893803621176636,-0.0872712977028124,
-0.0840071172452614,-0.0729063668309943,-0.0570412553575325,-0.0334066342075332,
-0.0265621740533172,-0.0225666130179622,-0.0190836151482547,-0.0155992334828168,
-0.00934406409815735,-0.000389160665116305),.UNSPECIFIED.);
#83=B_SPLINE_CURVE_WITH_KNOTS('',3,(#5944,#5945,#5946,#5947,#5948,#5949,
#5950,#5951,#5952,#5953,#5954,#5955,#5956,#5957,#5958,#5959,#5960,#5961),
 .UNSPECIFIED.,.F.,.F.,(4,2,2,2,2,2,2,2,4),(-1.72199006678857,-1.68750856578881,
-1.67979846079402,-1.67690108887121,-1.67485624629048,-1.67251384604177,
-1.6682564786429,-1.64426046576741,-1.64347692384346),.UNSPECIFIED.);
#84=B_SPLINE_CURVE_WITH_KNOTS('',3,(#5962,#5963,#5964,#5965,#5966,#5967,
#5968,#5969,#5970,#5971,#5972,#5973,#5974,#5975,#5976,#5977,#5978,#5979,
#5980,#5981,#5982,#5983,#5984,#5985,#5986,#5987,#5988,#5989,#5990,#5991,
#5992,#5993,#5994,#5995,#5996,#5997,#5998,#5999,#6000,#6001,#6002,#6003,
#6004,#6005,#6006,#6007,#6008,#6009,#6010,#6011,#6012,#6013,#6014,#6015,
#6016,#6017,#6018,#6019,#6020,#6021,#6022,#6023,#6024,#6025,#6026,#6027,
#6028,#6029,#6030,#6031,#6032,#6033,#6034,#6035,#6036,#6037,#6038,#6039,
#6040,#6041,#6042,#6043,#6044,#6045,#6046,#6047,#6048,#6049,#6050,#6051,
#6052,#6053,#6054,#6055,#6056,#6057,#6058,#6059,#6060,#6061,#6062,#6063,
#6064,#6065,#6066,#6067,#6068,#6069,#6070,#6071,#6072,#6073,#6074,#6075,
#6076,#6077,#6078,#6079,#6080,#6081,#6082,#6083,#6084,#6085,#6086,#6087,
#6088,#6089,#6090,#6091,#6092,#6093,#6094,#6095,#6096,#6097,#6098,#6099,
#6100,#6101,#6102,#6103,#6104,#6105,#6106,#6107,#6108,#6109,#6110,#6111,
#6112,#6113,#6114,#6115,#6116,#6117,#6118,#6119,#6120,#6121,#6122,#6123,
#6124,#6125,#6126,#6127,#6128,#6129,#6130,#6131,#6132,#6133,#6134,#6135,
#6136,#6137,#6138,#6139,#6140,#6141,#6142,#6143,#6144,#6145),
 .UNSPECIFIED.,.F.,.F.,(4,2,2,2,2,2,2,2,2,2,2,2,2,2,2,2,2,2,2,2,2,2,2,2,
2,2,2,2,2,2,2,2,2,2,2,2,2,2,2,2,2,2,2,2,2,2,2,2,2,2,2,2,2,2,2,2,2,2,2,2,
2,2,2,2,2,2,2,2,2,2,2,2,2,2,2,2,2,2,2,2,2,2,2,2,2,2,2,2,2,2,2,4),(-0.939896813873088,
-0.935945765197772,-0.931196725373738,-0.927594901368007,-0.923632744081659,
-0.916951051952594,-0.883448209138369,-0.867924648794366,-0.863619616212537,
-0.861292650799981,-0.859243809631339,-0.856317031658491,-0.848380786607831,
-0.834634699293341,-0.80413816353932,-0.79773557353793,-0.793829612153776,
-0.790209681130236,-0.785331084733207,-0.773263442024674,-0.753287587011472,
-0.732833061505069,-0.728386045506471,-0.726003594598022,-0.723968866668277,
-0.721146442191349,-0.713975648992959,-0.702283096907898,-0.671981201787048,
-0.663801840651034,-0.659497744422515,-0.655930940832998,-0.651665680332589,
-0.6434299070133,-0.63241295311361,-0.615882015096843,-0.597508309993198,
-0.593010316610334,-0.590617171529793,-0.588789050269151,-0.586119522556112,
-0.579948687960363,-0.540551986561062,-0.529833547112135,-0.525492806904551,
-0.521866569818422,-0.518060792777725,-0.512155294028801,-0.485106365917026,
-0.46182425897503,-0.457459482560063,-0.455094485793467,-0.453056031751265,
-0.45020319552216,-0.442816439523984,-0.430568141988818,-0.397961777612341,
-0.391499097539396,-0.387581134943543,-0.383965731841133,-0.379117307673376,
-0.367269696507562,-0.347938108162909,-0.326458349631957,-0.322063205476426,
-0.319691782589373,-0.317654823899299,-0.314813570848215,-0.307509462242839,
-0.295475799115584,-0.263776247764284,-0.256722849091742,-0.252647477038307,
-0.249426223290332,-0.245062685346377,-0.236287190473465,-0.224226337874599,
-0.208827257830432,-0.191157403554994,-0.18669978746137,-0.184315207104427,
-0.182485759572001,-0.179803891306055,-0.173556442487766,-0.138414739590681,
-0.124544267041282,-0.119326986104001,-0.115688662530475,-0.111902118200791,
-0.106093473042144,-0.0811916551463075,-0.0789957478678517),
 .UNSPECIFIED.);
#85=B_SPLINE_CURVE_WITH_KNOTS('',3,(#6150,#6151,#6152,#6153,#6154,#6155,
#6156,#6157,#6158,#6159,#6160,#6161,#6162,#6163,#6164,#6165,#6166,#6167,
#6168,#6169,#6170,#6171,#6172,#6173,#6174,#6175,#6176,#6177,#6178,#6179,
#6180,#6181,#6182,#6183,#6184,#6185,#6186,#6187,#6188,#6189,#6190,#6191,
#6192,#6193,#6194,#6195,#6196,#6197,#6198,#6199,#6200,#6201,#6202,#6203,
#6204,#6205,#6206,#6207,#6208,#6209,#6210,#6211,#6212,#6213,#6214,#6215,
#6216,#6217,#6218,#6219,#6220,#6221,#6222,#6223,#6224,#6225,#6226,#6227,
#6228,#6229,#6230,#6231,#6232,#6233,#6234,#6235,#6236,#6237,#6238,#6239,
#6240,#6241,#6242,#6243,#6244,#6245,#6246,#6247,#6248,#6249,#6250,#6251,
#6252,#6253,#6254,#6255,#6256,#6257,#6258,#6259,#6260,#6261,#6262,#6263,
#6264,#6265,#6266,#6267,#6268,#6269,#6270,#6271,#6272,#6273,#6274,#6275,
#6276,#6277,#6278,#6279,#6280,#6281,#6282,#6283,#6284,#6285,#6286,#6287,
#6288,#6289,#6290,#6291,#6292,#6293,#6294,#6295,#6296,#6297,#6298,#6299,
#6300,#6301,#6302,#6303,#6304,#6305,#6306,#6307,#6308,#6309,#6310,#6311,
#6312,#6313,#6314,#6315,#6316,#6317,#6318,#6319,#6320,#6321,#6322,#6323,
#6324,#6325),.UNSPECIFIED.,.F.,.F.,(4,2,2,2,2,2,2,2,2,2,2,2,2,2,2,2,2,2,
2,2,2,2,2,2,2,2,2,2,2,2,2,2,2,2,2,2,2,2,2,2,2,2,2,2,2,2,2,2,2,2,2,2,2,2,
2,2,2,2,2,2,2,2,2,2,2,2,2,2,2,2,2,2,2,2,2,2,2,2,2,2,2,2,2,2,2,2,2,4),(-1.6432613616363,
-1.64161314158455,-1.63517065096013,-1.60035856750064,-1.58937151171928,
-1.58249256221114,-1.57972586961991,-1.57772343305823,-1.5753312885874,
-1.57084086371976,-1.55256684156769,-1.53154503040702,-1.51867274857762,
-1.51368160165886,-1.51003665769862,-1.50615656624993,-1.49991602379275,
-1.46836947911062,-1.45527948874169,-1.44757813600774,-1.44467514664117,
-1.44262403943427,-1.44027334731779,-1.43598400490242,-1.41227202807211,
-1.38547443452719,-1.37963909308575,-1.37584654743783,-1.372210344127,-1.36783009767956,
-1.35685020234345,-1.31769060898488,-1.31155745259713,-1.30889466424372,
-1.30706835165882,-1.30467412953405,-1.30016449476984,-1.28162684568544,
-1.26041571902772,-1.24795152497195,-1.24302348340268,-1.23939905236228,
-1.23551818339787,-1.22922717130057,-1.19785438429616,-1.18453439255849,
-1.17675119962063,-1.17384617561964,-1.17180159898918,-1.1694651807813,
-1.16523553718916,-1.14077067859652,-1.12326672460158,-1.11208500468429,
-1.10732972618432,-1.10372542174437,-1.0997625818622,-1.09308431529482,
-1.0655092196304,-1.0501006604258,-1.04160731553292,-1.03860962029435,-1.03654884428248,
-1.03425237835456,-1.03009686526669,-1.00408785176088,-0.9791741946859,
-0.973366700081466,-0.969580258348652,-0.965941500253462,-0.960722629720811,
-0.946865847082279,-0.911692371408435,-0.905437735994771,-0.90275472786554,
-0.900925220596629,-0.898541510757078,-0.894087837670476,-0.876489006982961,
-0.861280684840634,-0.843337904312691,-0.837733808194014,-0.834361243892084,
-0.830708020484245,-0.825617005449271,-0.811845733161868,-0.78583367335449,
-0.782599245859888),.UNSPECIFIED.);
#86=B_SPLINE_CURVE_WITH_KNOTS('',3,(#6327,#6328,#6329,#6330,#6331,#6332,
#6333,#6334,#6335,#6336,#6337,#6338,#6339,#6340,#6341,#6342),
 .UNSPECIFIED.,.F.,.F.,(4,2,2,2,2,2,2,4),(-0.0789957478678517,-0.0551148295329374,
-0.0509626629422434,-0.0486671676406389,-0.0466076700700712,-0.0436120653051043,
-0.0351252602160147,-0.000467694393496468),.UNSPECIFIED.);
#87=B_SPLINE_CURVE_WITH_KNOTS('',3,(#6343,#6344,#6345,#6346,#6347,#6348,
#6349,#6350,#6351,#6352,#6353,#6354,#6355,#6356,#6357,#6358,#6359,#6360,
#6361,#6362,#6363,#6364,#6365,#6366,#6367,#6368,#6369,#6370,#6371,#6372,
#6373,#6374,#6375,#6376,#6377,#6378,#6379,#6380,#6381,#6382,#6383,#6384,
#6385,#6386,#6387,#6388,#6389,#6390,#6391,#6392,#6393,#6394,#6395,#6396,
#6397,#6398,#6399,#6400,#6401,#6402,#6403,#6404,#6405,#6406,#6407,#6408,
#6409,#6410,#6411,#6412,#6413,#6414,#6415,#6416,#6417,#6418,#6419,#6420,
#6421,#6422,#6423,#6424,#6425,#6426,#6427,#6428,#6429,#6430,#6431,#6432,
#6433,#6434,#6435,#6436,#6437,#6438,#6439,#6440,#6441,#6442,#6443,#6444,
#6445,#6446,#6447,#6448,#6449,#6450,#6451,#6452,#6453,#6454,#6455,#6456,
#6457,#6458,#6459,#6460,#6461,#6462,#6463,#6464,#6465,#6466,#6467,#6468,
#6469,#6470,#6471,#6472,#6473,#6474,#6475,#6476,#6477,#6478,#6479,#6480,
#6481,#6482,#6483,#6484,#6485,#6486,#6487,#6488,#6489,#6490,#6491,#6492,
#6493,#6494,#6495,#6496,#6497,#6498,#6499,#6500,#6501,#6502,#6503,#6504,
#6505,#6506,#6507,#6508,#6509,#6510),.UNSPECIFIED.,.F.,.F.,(4,2,2,2,2,2,
2,2,2,2,2,2,2,2,2,2,2,2,2,2,2,2,2,2,2,2,2,2,2,2,2,2,2,2,2,2,2,2,2,2,2,2,
2,2,2,2,2,2,2,2,2,2,2,2,2,2,2,2,2,2,2,2,2,2,2,2,2,2,2,2,2,2,2,2,2,2,2,2,
2,2,2,2,2,4),(0.782675134033573,0.782757485927756,0.79475868109047,0.798176777831719,
0.800104431433756,0.802211228332774,0.805465846820559,0.816456368900843,
0.842152606133684,0.858697906830614,0.864240310369191,0.867603266628399,
0.871266977594691,0.876412828561605,0.890664055646709,0.918913849486384,
0.930243122109789,0.933609935042696,0.935530065740048,0.937648381135311,
0.940958897741722,0.952617221264153,0.982558786625348,0.995139239295908,
1.00021136792272,1.00382517622462,1.00765269196997,1.0136675642461,1.03885136040049,
1.06405934903704,1.06824645506887,1.07057318495682,1.07262140621808,1.07554680049778,
1.08347506120726,1.09720008463773,1.12776711776842,1.13416346016404,1.13806759007756,
1.14168703025469,1.14656681390693,1.15864939288267,1.17867289197161,1.19898414322743,
1.20345332047464,1.20584010470427,1.20766893530967,1.21034680925492,1.2165696116661,
1.25162358005158,1.26561408639473,1.27084423366087,1.27448474097013,1.27826786510143,
1.2840595405384,1.30830424262765,1.33520506211329,1.33925760994492,1.34153239052917,
1.34360017810509,1.34664599470362,1.35556049046178,1.37233653973675,1.39793017143743,
1.40467342657647,1.40864778588906,1.41224606448015,1.41696895461105,1.42794269808721,
1.44491431607832,1.4703072739279,1.4744777338303,1.47680092931909,1.47885045329991,
1.481783835504,1.48977297224307,1.51117459842206,1.53323974042741,1.54002851148807,
1.5440120563922,1.54748826067801,1.55097547824573,1.55683902380664,1.56494898091576),
 .UNSPECIFIED.);
#88=B_SPLINE_CURVE_WITH_KNOTS('',3,(#6514,#6515,#6516,#6517,#6518,#6519),
 .UNSPECIFIED.,.F.,.F.,(4,1,1,4),(-4.09232582034257,-3.95356055398286,-2.96517041548714,
-2.06969806661986),.UNSPECIFIED.);
#89=B_SPLINE_CURVE_WITH_KNOTS('',3,(#6523,#6524,#6525,#6526,#6527),
 .UNSPECIFIED.,.F.,.F.,(4,1,4),(0.,0.988390138495704,1.11850960794437),
 .UNSPECIFIED.);
#90=B_SPLINE_CURVE_WITH_KNOTS('',3,(#6529,#6530,#6531,#6532,#6533,#6534,
#6535,#6536,#6537,#6538,#6539,#6540,#6541,#6542,#6543,#6544,#6545,#6546,
#6547,#6548,#6549,#6550,#6551,#6552,#6553,#6554,#6555,#6556,#6557,#6558,
#6559,#6560,#6561,#6562,#6563,#6564,#6565,#6566,#6567,#6568,#6569,#6570,
#6571,#6572,#6573,#6574,#6575,#6576,#6577,#6578,#6579,#6580,#6581,#6582,
#6583,#6584,#6585,#6586,#6587,#6588,#6589,#6590,#6591,#6592,#6593,#6594,
#6595,#6596,#6597,#6598,#6599,#6600,#6601,#6602,#6603,#6604,#6605,#6606,
#6607,#6608,#6609,#6610,#6611,#6612,#6613,#6614,#6615,#6616,#6617,#6618,
#6619,#6620,#6621,#6622,#6623,#6624,#6625,#6626,#6627,#6628,#6629,#6630,
#6631,#6632,#6633,#6634,#6635,#6636,#6637,#6638,#6639,#6640,#6641,#6642,
#6643,#6644,#6645,#6646,#6647,#6648,#6649,#6650,#6651,#6652,#6653,#6654,
#6655,#6656,#6657,#6658,#6659,#6660,#6661,#6662,#6663,#6664,#6665,#6666,
#6667,#6668,#6669,#6670,#6671,#6672,#6673,#6674,#6675,#6676,#6677,#6678,
#6679,#6680,#6681,#6682,#6683,#6684,#6685,#6686,#6687,#6688,#6689,#6690,
#6691,#6692,#6693,#6694,#6695,#6696,#6697,#6698,#6699,#6700,#6701,#6702,
#6703),.UNSPECIFIED.,.F.,.F.,(4,3,3,3,3,3,3,3,3,3,3,3,3,3,3,3,3,3,3,3,3,
3,3,3,3,3,3,3,3,3,3,3,3,3,3,3,3,3,3,3,3,3,3,3,3,3,3,3,3,3,3,3,3,3,3,3,3,
3,4),(1.11850960794437,1.22579344157525,1.33223603590235,1.43859406334533,
1.54491030815538,1.65287780036439,1.75930425580786,1.86804226639964,1.97678027699142,
2.08619472520565,2.19606668649083,2.30518861914641,2.41424528619025,2.52327607349202,
2.6337496589908,2.74291250415898,2.85404145982306,2.96517041548714,3.07458685153405,
3.18445856434015,3.29359150555844,3.4026625541112,3.51171108558613,3.62217345268532,
3.73136219092843,3.84246137245565,3.95356055398286,4.06264813384511,4.1725609536743,
4.2813505245247,4.39007374209031,4.49877057062825,4.60956560109083,4.71839716172489,
4.83017392710173,4.94195069247857,5.05122246113134,5.16111225736171,5.27009152387901,
5.37900596450968,5.48789522451555,5.59850662613023,5.70753138898118,5.81893610997773,
5.93034083097429,6.03959681195816,6.14948858164714,6.25845280370696,6.36735252397173,
6.47622741436736,6.58685330314302,6.69586473711608,6.80729785329305,6.91873096947001,
7.0394719557711,7.15440370853321,7.26911755665986,7.38356740485535,7.40169491467437),
 .UNSPECIFIED.);
#91=B_SPLINE_CURVE_WITH_KNOTS('',3,(#6705,#6706,#6707,#6708,#6709,#6710,
#6711,#6712,#6713,#6714,#6715,#6716,#6717,#6718,#6719,#6720,#6721,#6722,
#6723,#6724,#6725,#6726,#6727,#6728,#6729,#6730,#6731,#6732,#6733,#6734,
#6735,#6736,#6737,#6738,#6739,#6740,#6741,#6742,#6743,#6744,#6745,#6746,
#6747,#6748,#6749,#6750,#6751,#6752,#6753,#6754,#6755,#6756,#6757,#6758,
#6759,#6760,#6761,#6762,#6763,#6764,#6765,#6766,#6767,#6768,#6769,#6770,
#6771,#6772,#6773,#6774,#6775,#6776,#6777,#6778,#6779,#6780,#6781,#6782,
#6783,#6784,#6785,#6786,#6787,#6788,#6789,#6790,#6791,#6792,#6793,#6794,
#6795,#6796,#6797,#6798,#6799,#6800,#6801,#6802,#6803,#6804,#6805,#6806,
#6807,#6808,#6809,#6810,#6811,#6812,#6813,#6814,#6815,#6816,#6817,#6818,
#6819,#6820,#6821,#6822,#6823,#6824,#6825,#6826,#6827,#6828,#6829,#6830,
#6831,#6832,#6833,#6834,#6835,#6836,#6837,#6838,#6839,#6840,#6841,#6842,
#6843,#6844,#6845,#6846,#6847,#6848,#6849,#6850,#6851,#6852,#6853,#6854,
#6855,#6856,#6857,#6858,#6859,#6860,#6861,#6862,#6863,#6864,#6865,#6866,
#6867,#6868,#6869,#6870,#6871,#6872,#6873,#6874,#6875,#6876,#6877,#6878,
#6879),.UNSPECIFIED.,.F.,.F.,(4,3,3,3,3,3,3,3,3,3,3,3,3,3,3,3,3,3,3,3,3,
3,3,3,3,3,3,3,3,3,3,3,3,3,3,3,3,3,3,3,3,3,3,3,3,3,3,3,3,3,3,3,3,3,3,3,3,
3,4),(7.40169491512396,7.51508585839002,7.62876448289629,7.74259833580656,
7.85672333604955,7.90712110796573,8.01636379034547,8.12625722235997,8.23520710733033,
8.34409214137705,8.45295202069422,8.56359182713602,8.67258761935882,8.78404943291013,
8.89551124646144,9.0047489895559,9.11464303898106,9.2235879892422,9.33246810470449,
9.44132309010251,9.55196766381617,9.66095868084071,9.77243003289893,9.88390138495715,
9.99313410876066,10.1030287855972,10.2119684564921,10.3208432100475,10.4296927599658,
10.5403424508376,10.6493279132887,10.7608097183708,10.8722915234529,10.9815285124691,
11.091422656154,11.200366741289,11.3092459523339,11.4180999954536,11.5287454120773,
11.6377354037949,11.7492085328717,11.8606816619486,11.9699175713013,12.0798118499442,
12.1887548410624,12.2976329558757,12.4064859024314,12.5171323769346,12.6261212841214,
12.7375965422828,12.8490718004443,12.9566773999038,13.0641381618935,13.1714962465973,
13.2787936552669,13.3861279145202,13.4934766413414,13.6009727981548,13.6848802223035),
 .UNSPECIFIED.);
#92=B_SPLINE_CURVE_WITH_KNOTS('',3,(#6881,#6882,#6883,#6884,#6885,#6886,
#6887,#6888,#6889,#6890,#6891),.UNSPECIFIED.,.F.,.F.,(4,1,1,1,1,1,1,1,4),
(13.6848802223035,13.83746193894,14.8258520774357,15.8142422159314,16.8026323544271,
17.7910224929229,18.7794126314186,19.7678027699143,19.9680655294831),
 .UNSPECIFIED.);
#93=B_SPLINE_CURVE_WITH_KNOTS('',3,(#6893,#6894,#6895,#6896,#6897,#6898,
#6899,#6900,#6901,#6902),.UNSPECIFIED.,.F.,.F.,(4,1,1,1,1,1,1,4),(19.9680655294831,
20.75619290841,21.7445830469057,22.7329731854014,23.7213633238971,24.7097534623929,
25.6981436008886,26.2512508366627),.UNSPECIFIED.);
#94=B_SPLINE_CURVE_WITH_KNOTS('',3,(#6904,#6905,#6906,#6907,#6908,#6909,
#6910,#6911,#6912,#6913),.UNSPECIFIED.,.F.,.F.,(4,1,1,1,1,1,1,4),(26.2512508366627,
26.6865337393843,27.67492387788,28.6633140163757,29.6517041548714,30.6400942933671,
31.6284844318629,32.5344361438423),.UNSPECIFIED.);
#95=B_SPLINE_CURVE_WITH_KNOTS('',3,(#6915,#6916,#6917,#6918,#6919,#6920,
#6921,#6922,#6923,#6924,#6925),.UNSPECIFIED.,.F.,.F.,(4,1,1,1,1,1,1,1,4),
(32.5344361438423,32.6168745703586,33.6052647088543,34.59365484735,35.5820449858457,
36.5704351243414,37.5588252628371,38.5472154013329,38.8176214510219),
 .UNSPECIFIED.);
#96=B_SPLINE_CURVE_WITH_KNOTS('',3,(#6927,#6928,#6929,#6930,#6931,#6932,
#6933,#6934,#6935,#6936),.UNSPECIFIED.,.F.,.F.,(4,1,1,1,1,1,1,4),(38.8176214510219,
39.5356055398286,40.5239956783243,41.51238581682,42.5007759553157,43.4891660938114,
44.4775562323071,45.1008067582015),.UNSPECIFIED.);
#97=B_SPLINE_CURVE_WITH_KNOTS('',3,(#6938,#6939,#6940,#6941,#6942,#6943,
#6944,#6945,#6946,#6947),.UNSPECIFIED.,.F.,.F.,(4,1,1,1,1,1,1,4),(45.1008067582015,
45.4659463708029,46.4543365092986,47.4427266477943,48.43111678629,49.4195069247857,
50.4078970632814,51.3839920653811),.UNSPECIFIED.);
#98=B_SPLINE_CURVE_WITH_KNOTS('',3,(#6949,#6950,#6951,#6952,#6953,#6954,
#6955,#6956,#6957,#6958,#6959,#6960),.UNSPECIFIED.,.F.,.F.,(4,2,1,1,1,1,
1,1,4),(51.3839920653811,51.3962872017771,52.3846773402729,53.3730674787686,
54.3614576172643,55.34984775576,56.3382378942557,57.3266280327514,57.6671773725607),
 .UNSPECIFIED.);
#99=B_SPLINE_CURVE_WITH_KNOTS('',3,(#6962,#6963,#6964,#6965,#6966,#6967,
#6968,#6969,#6970,#6971),.UNSPECIFIED.,.F.,.F.,(4,1,1,1,1,1,1,4),(57.6671773725607,
58.3150181712471,59.3034083097429,60.2917984482386,61.2801885867343,62.26857872523,
63.2569688637257,63.9503626797403),.UNSPECIFIED.);
#100=B_SPLINE_CURVE_WITH_KNOTS('',3,(#6973,#6974,#6975,#6976,#6977,#6978,
#6979,#6980,#6981,#6982,#6983),.UNSPECIFIED.,.F.,.F.,(4,1,1,1,1,1,1,1,4),
(63.9503626797403,64.2453590022215,65.2337491407172,66.2221392792129,67.2105294177086,
68.1989195562043,69.1873096947,70.1756998331957,70.2335479869199),
 .UNSPECIFIED.);
#101=B_SPLINE_CURVE_WITH_KNOTS('',3,(#6985,#6986,#6987,#6988,#6989),
 .UNSPECIFIED.,.F.,.F.,(4,1,4),(70.2335479869199,71.1640899716914,72.0600176124814),
 .UNSPECIFIED.);
#102=B_SPLINE_CURVE_WITH_KNOTS('',3,(#6993,#6994,#6995,#6996,#6997,#6998,
#6999,#7000,#7001,#7002,#7003,#7004,#7005,#7006,#7007,#7008,#7009,#7010,
#7011,#7012,#7013,#7014,#7015,#7016,#7017,#7018,#7019,#7020),
 .UNSPECIFIED.,.F.,.F.,(4,3,3,3,3,3,3,3,3,4),(-74.1292603871786,-74.014023363696,
-73.9035575273749,-73.7931227076102,-73.6826829382937,-73.5722022608866,
-73.4615630851229,-73.3508315426675,-73.2398888203009,-73.2073641993181),
 .UNSPECIFIED.);
#103=B_SPLINE_CURVE_WITH_KNOTS('',3,(#7022,#7023,#7024,#7025,#7026,#7027,
#7028,#7029,#7030,#7031,#7032),.UNSPECIFIED.,.F.,.F.,(4,1,1,1,1,1,1,1,4),
(-73.2073641993181,-73.1408702486829,-72.1524801101872,-71.1640899716915,
-70.1756998331958,-69.1873096947,-68.1989195562043,-67.2105294177086,-66.9241788921385),
 .UNSPECIFIED.);
#104=B_SPLINE_CURVE_WITH_KNOTS('',3,(#7034,#7035,#7036,#7037,#7038,#7039,
#7040,#7041,#7042,#7043),.UNSPECIFIED.,.F.,.F.,(4,1,1,1,1,1,1,4),(-66.9241788921385,
-66.2221392792129,-65.2337491407172,-64.2453590022215,-63.2569688637258,
-62.26857872523,-61.2801885867343,-60.6409935849589),.UNSPECIFIED.);
#105=B_SPLINE_CURVE_WITH_KNOTS('',3,(#7045,#7046,#7047,#7048,#7049,#7050,
#7051,#7052,#7053,#7054,#7055),.UNSPECIFIED.,.F.,.F.,(4,1,1,1,1,1,1,1,4),
(-60.6409935849589,-60.2917984482386,-59.3034083097429,-58.3150181712472,
-57.3266280327515,-56.3382378942557,-55.34984775576,-54.3614576172643,-54.3578082777793),
 .UNSPECIFIED.);
#106=B_SPLINE_CURVE_WITH_KNOTS('',3,(#7057,#7058,#7059,#7060,#7061,#7062,
#7063,#7064,#7065,#7066),.UNSPECIFIED.,.F.,.F.,(4,1,1,1,1,1,1,4),(-54.3578082777793,
-53.3730674787686,-52.3846773402729,-51.3962872017772,-50.4078970632814,
-49.4195069247857,-48.43111678629,-48.0746229705997),.UNSPECIFIED.);
#107=B_SPLINE_CURVE_WITH_KNOTS('',3,(#7068,#7069,#7070,#7071,#7072,#7073,
#7074,#7075,#7076,#7077),.UNSPECIFIED.,.F.,.F.,(4,1,1,1,1,1,1,4),(-48.0746229705997,
-47.4427266477943,-46.4543365092986,-45.4659463708029,-44.4775562323072,
-43.4891660938114,-42.5007759553157,-41.7914376634201),.UNSPECIFIED.);
#108=B_SPLINE_CURVE_WITH_KNOTS('',3,(#7079,#7080,#7081,#7082,#7083,#7084,
#7085,#7086,#7087,#7088,#7089),.UNSPECIFIED.,.F.,.F.,(4,1,1,1,1,1,1,1,4),
(-41.7914376634201,-41.51238581682,-40.5239956783243,-39.5356055398286,
-38.5472154013329,-37.5588252628372,-36.5704351243414,-35.5820449858457,
-35.5082523562405),.UNSPECIFIED.);
#109=B_SPLINE_CURVE_WITH_KNOTS('',3,(#7091,#7092,#7093,#7094,#7095,#7096,
#7097,#7098,#7099,#7100),.UNSPECIFIED.,.F.,.F.,(4,1,1,1,1,1,1,4),(-35.5082523562405,
-34.59365484735,-33.6052647088543,-32.6168745703586,-31.6284844318629,-30.6400942933672,
-29.6517041548714,-29.2250670490609),.UNSPECIFIED.);
#110=B_SPLINE_CURVE_WITH_KNOTS('',3,(#7102,#7103,#7104,#7105,#7106,#7107,
#7108,#7109,#7110,#7111),.UNSPECIFIED.,.F.,.F.,(4,1,1,1,1,1,1,4),(-29.2250670490609,
-28.6633140163757,-27.67492387788,-26.6865337393843,-25.6981436008886,-24.7097534623929,
-23.7213633238972,-22.9418817418813),.UNSPECIFIED.);
#111=B_SPLINE_CURVE_WITH_KNOTS('',3,(#7113,#7114,#7115,#7116,#7117,#7118,
#7119,#7120,#7121,#7122,#7123),.UNSPECIFIED.,.F.,.F.,(4,1,1,1,1,1,1,1,4),
(-22.9418817418813,-22.7329731854014,-21.7445830469057,-20.75619290841,
-19.7678027699143,-18.7794126314186,-17.7910224929229,-16.8026323544271,
-16.6586964347017),.UNSPECIFIED.);
#112=B_SPLINE_CURVE_WITH_KNOTS('',3,(#7125,#7126,#7127,#7128,#7129,#7130,
#7131,#7132,#7133,#7134),.UNSPECIFIED.,.F.,.F.,(4,1,1,1,1,1,1,4),(-16.6586964347017,
-15.8142422159314,-14.8258520774357,-13.83746193894,-12.8490718004443,-11.8606816619486,
-10.8722915234529,-10.3755111275222),.UNSPECIFIED.);
#113=B_SPLINE_CURVE_WITH_KNOTS('',3,(#7135,#7136,#7137,#7138,#7139,#7140,
#7141,#7142,#7143,#7144,#7145,#7146,#7147,#7148,#7149,#7150,#7151,#7152,
#7153,#7154,#7155,#7156,#7157,#7158,#7159,#7160,#7161,#7162,#7163,#7164,
#7165,#7166,#7167,#7168,#7169,#7170,#7171,#7172,#7173,#7174,#7175,#7176,
#7177,#7178,#7179,#7180,#7181,#7182,#7183,#7184,#7185,#7186,#7187,#7188,
#7189,#7190,#7191,#7192,#7193,#7194,#7195,#7196,#7197,#7198,#7199,#7200,
#7201,#7202,#7203,#7204,#7205,#7206,#7207,#7208,#7209,#7210,#7211,#7212,
#7213,#7214,#7215,#7216,#7217,#7218,#7219,#7220,#7221,#7222,#7223,#7224,
#7225,#7226,#7227,#7228,#7229,#7230,#7231,#7232,#7233,#7234,#7235,#7236,
#7237,#7238,#7239,#7240,#7241,#7242,#7243,#7244,#7245,#7246,#7247,#7248,
#7249,#7250,#7251,#7252,#7253,#7254,#7255,#7256,#7257,#7258,#7259,#7260,
#7261,#7262,#7263,#7264,#7265,#7266,#7267,#7268,#7269,#7270,#7271,#7272,
#7273,#7274,#7275,#7276,#7277,#7278,#7279,#7280,#7281,#7282,#7283,#7284,
#7285,#7286,#7287,#7288,#7289,#7290,#7291,#7292,#7293,#7294,#7295,#7296,
#7297,#7298,#7299,#7300,#7301,#7302,#7303,#7304,#7305,#7306,#7307,#7308,
#7309),.UNSPECIFIED.,.F.,.F.,(4,3,3,3,3,3,3,3,3,3,3,3,3,3,3,3,3,3,3,3,3,
3,3,3,3,3,3,3,3,3,3,3,3,3,3,3,3,3,3,3,3,3,3,3,3,3,3,3,3,3,3,3,3,3,3,3,3,
3,4),(-10.3755111025761,-10.2614689943702,-10.1471056802317,-10.0325664532904,
-9.91772759343654,-9.88390138495715,-9.77466328603903,-9.66476928109183,
-9.55582418286387,-9.446943997502,-9.33808902015295,-9.22744457673007,-9.11845375896544,
-9.00698250271344,-8.89551124646144,-8.78626851305079,-8.67637508741516,
-8.56742517260818,-8.45854011672707,-8.34968022359019,-8.23904044468407,
-8.13004465846976,-8.01858288321774,-7.90712110796572,-7.79790831958831,
-7.68801115082352,-7.57909129493945,-7.47023625590901,-7.36140628774901,
-7.25073745817926,-7.14177102748603,-7.03025099847802,-6.91873096947,-6.80947225831212,
-6.69958082989489,-6.59061547220279,-6.48171521526574,-6.37284038625179,
-6.26221549743242,-6.15320559159024,-6.04177321128226,-5.93034083097429,
-5.82106975234147,-5.71117986985861,-5.60220084897479,-5.49328648723783,
-5.38439713975623,-5.27378552793682,-5.16476027045818,-5.05335548146837,
-4.94195069247857,-4.83445286275916,-4.72709981013473,-4.61984927129259,
-4.51265914426547,-4.40542736627408,-4.29818096566019,-4.19077482677967,
-4.09232582034257),.UNSPECIFIED.);
#114=B_SPLINE_CURVE_WITH_KNOTS('',3,(#7312,#7313,#7314,#7315,#7316,#7317,
#7318,#7319,#7320,#7321,#7322,#7323,#7324,#7325,#7326,#7327,#7328,#7329,
#7330,#7331,#7332,#7333,#7334,#7335,#7336,#7337,#7338,#7339,#7340,#7341,
#7342,#7343,#7344,#7345,#7346,#7347,#7348,#7349,#7350,#7351,#7352,#7353,
#7354,#7355,#7356,#7357,#7358,#7359,#7360,#7361,#7362,#7363,#7364,#7365,
#7366,#7367,#7368,#7369,#7370,#7371,#7372,#7373,#7374,#7375,#7376,#7377,
#7378,#7379,#7380,#7381,#7382,#7383,#7384,#7385,#7386,#7387,#7388,#7389,
#7390,#7391,#7392,#7393,#7394,#7395,#7396,#7397,#7398,#7399,#7400,#7401,
#7402,#7403,#7404,#7405,#7406,#7407,#7408,#7409,#7410,#7411,#7412,#7413,
#7414,#7415,#7416,#7417,#7418,#7419,#7420,#7421,#7422,#7423,#7424,#7425,
#7426,#7427,#7428,#7429,#7430,#7431,#7432,#7433,#7434,#7435,#7436,#7437,
#7438,#7439,#7440,#7441,#7442,#7443,#7444,#7445,#7446,#7447,#7448,#7449,
#7450,#7451,#7452,#7453,#7454,#7455,#7456,#7457,#7458,#7459,#7460,#7461,
#7462,#7463,#7464,#7465),.UNSPECIFIED.,.F.,.F.,(4,2,2,2,2,2,2,2,2,2,2,2,
2,2,2,2,2,2,2,2,2,2,2,2,2,2,2,2,2,2,2,2,2,2,2,2,2,2,2,2,2,2,2,2,2,2,2,2,
2,2,2,2,2,2,2,2,2,2,2,2,2,2,2,2,2,2,2,2,2,2,2,2,2,2,2,2,4),(0.0019271125636388,
0.0359882586975409,0.0488495312971493,0.053884776286046,0.0575798993696898,
0.061533608308059,0.0679528681421754,0.09694686298088,0.110574076667147,
0.118468402614831,0.121437295887913,0.123533451649698,0.125924118639411,
0.130471602975681,0.151602133207587,0.170896061494497,0.182719350336417,
0.187575881186773,0.191205611514928,0.195147824979162,0.201672627265219,
0.231619614775219,0.245840725214441,0.251413458609416,0.255672786850559,
0.257990756854425,0.260031973366808,0.262954354156453,0.270390438492984,
0.29405438915914,0.316492447629417,0.322202831441264,0.32595083015959,0.329568877776729,
0.33395574597341,0.345268569245878,0.384140969187585,0.390289845099253,
0.392943121292912,0.39476247355183,0.397149705141244,0.401616678980508,
0.419464108466401,0.44127771261733,0.453941340636418,0.458906304353505,
0.462547142592922,0.466436528546787,0.472723312330512,0.503918813642895,
0.517174552285323,0.524936547689952,0.527847585423213,0.529899856004968,
0.53224623173506,0.536515539926699,0.566259134935688,0.585849849580721,
0.592322830082281,0.596243357140048,0.599858860622756,0.604619302853052,
0.615285948369656,0.654774978012272,0.660979991486942,0.663654313514544,
0.66548177482559,0.667867512905708,0.672337417126603,0.692659143088369,
0.719694546424965,0.727100056009227,0.731203617792598,0.734774906305486,
0.739265237973076,0.748788247652177,0.782675134033573),.UNSPECIFIED.);
#115=B_SPLINE_CURVE_WITH_KNOTS('',3,(#7469,#7470,#7471,#7472,#7473,#7474,
#7475,#7476,#7477,#7478,#7479,#7480,#7481,#7482,#7483,#7484,#7485,#7486,
#7487,#7488,#7489,#7490,#7491,#7492,#7493,#7494,#7495,#7496,#7497,#7498,
#7499,#7500,#7501,#7502,#7503,#7504,#7505,#7506,#7507,#7508,#7509,#7510,
#7511,#7512,#7513,#7514,#7515,#7516,#7517,#7518,#7519,#7520,#7521,#7522,
#7523,#7524,#7525,#7526,#7527,#7528,#7529,#7530,#7531,#7532,#7533,#7534,
#7535,#7536,#7537,#7538,#7539,#7540,#7541,#7542,#7543,#7544,#7545,#7546,
#7547,#7548,#7549,#7550,#7551,#7552,#7553,#7554,#7555,#7556,#7557,#7558,
#7559,#7560,#7561,#7562,#7563,#7564,#7565,#7566,#7567,#7568,#7569,#7570,
#7571,#7572,#7573,#7574),.UNSPECIFIED.,.F.,.F.,(4,3,3,3,3,3,3,3,3,3,3,3,
3,3,3,3,3,3,3,3,3,3,3,3,3,3,3,3,3,3,3,3,3,3,3,4),(78.5398163401459,78.6561340881922,
78.7706355519136,78.8850310411815,78.9993690019213,79.11711633257,79.2315565783168,
79.3509574514166,79.4703583245163,79.5860523177359,79.7015449273291,79.8169263900411,
79.9322433694907,80.0475424284951,80.1629505027753,80.2784173412434,80.3940938012417,
80.458748463012,80.5730139624223,80.6870758225365,80.8010260233051,80.9149135960265,
81.028787466322,81.1427876464366,81.2568539755108,81.3711583644439,81.4471386015078,
81.5706873688198,81.6891165335582,81.8073967935847,81.925566265604,82.0436628949241,
82.1617581236453,82.2798497928827,82.3980223100823,82.4355287400035),
 .UNSPECIFIED.);
#116=B_SPLINE_CURVE_WITH_KNOTS('',3,(#7575,#7576,#7577,#7578,#7579,#7580,
#7581,#7582,#7583,#7584,#7585,#7586,#7587,#7588,#7589,#7590,#7591,#7592,
#7593,#7594,#7595,#7596,#7597,#7598),.UNSPECIFIED.,.F.,.F.,(4,2,2,2,2,2,
2,2,2,2,2,4),(-1.72176609592119,-1.71857158954466,-1.71581859485177,-1.7139477611094,
-1.71180394756969,-1.70832902031807,-1.69506735904276,-1.66549716493993,
-1.65388885134957,-1.64909455131773,-1.64550843441701,-1.6432613616363),
 .UNSPECIFIED.);
#117=B_SPLINE_CURVE_WITH_KNOTS('',3,(#7911,#7912,#7913,#7914,#7915,#7916,
#7917,#7918,#7919,#7920,#7921,#7922,#7923,#7924,#7925,#7926,#7927,#7928,
#7929,#7930,#7931,#7932,#7933,#7934,#7935,#7936,#7937,#7938,#7939,#7940,
#7941,#7942,#7943,#7944,#7945,#7946,#7947,#7948,#7949,#7950,#7951,#7952,
#7953,#7954,#7955,#7956,#7957,#7958,#7959,#7960,#7961,#7962,#7963,#7964,
#7965,#7966,#7967,#7968,#7969,#7970,#7971,#7972,#7973,#7974,#7975,#7976,
#7977,#7978,#7979,#7980,#7981,#7982,#7983,#7984,#7985,#7986,#7987,#7988,
#7989),.UNSPECIFIED.,.F.,.F.,(4,3,3,3,3,3,3,3,3,3,3,3,3,3,3,3,3,3,3,3,3,
3,3,3,3,3,4),(-0.319964203083861,-0.304228037518007,-0.284613148690911,
-0.276871331371113,-0.272257224906624,-0.252969211159584,-0.239387034404623,
-0.231434900380484,-0.227996911242295,-0.209251097418081,-0.190531504790305,
-0.171811912162528,-0.167655673991812,-0.1499077162788,-0.144306654204072,
-0.125663099898434,-0.11745065284486,-0.112094758046013,-0.10874239451909,
-0.0911202044344707,-0.0736624604297992,-0.0563420615200763,-0.0520648001853392,
-0.0351733175045267,-0.0188296765697835,-0.00258365319679502,0.),
 .UNSPECIFIED.);
#118=B_SPLINE_CURVE_WITH_KNOTS('',3,(#7990,#7991,#7992,#7993,#7994,#7995,
#7996,#7997,#7998,#7999,#8000,#8001,#8002,#8003,#8004,#8005,#8006,#8007,
#8008,#8009,#8010,#8011,#8012,#8013,#8014,#8015,#8016,#8017,#8018,#8019,
#8020,#8021,#8022,#8023,#8024,#8025,#8026,#8027,#8028,#8029,#8030,#8031,
#8032,#8033,#8034,#8035,#8036,#8037,#8038,#8039,#8040,#8041,#8042,#8043,
#8044,#8045,#8046,#8047,#8048,#8049,#8050,#8051,#8052,#8053,#8054,#8055,
#8056,#8057,#8058,#8059,#8060,#8061,#8062,#8063,#8064,#8065,#8066,#8067,
#8068,#8069,#8070,#8071),.UNSPECIFIED.,.F.,.F.,(4,3,3,3,3,3,3,3,3,3,3,3,
3,3,3,3,3,3,3,3,3,3,3,3,3,3,3,4),(0.,0.0128150276685244,0.0291235486693142,
0.0458461102161369,0.052840853654919,0.0569615705457033,0.0648285591165465,
0.0821842191184943,0.0998369062260194,0.108571225247779,0.112969449381281,
0.131127949227731,0.149229095291533,0.158622885237427,0.169525023140723,
0.17289105881689,0.190819970311636,0.209351312635224,0.223582858937968,
0.228841969886222,0.234245615182723,0.253464440755347,0.269667484046342,
0.274196754530456,0.277710493273208,0.297309565454661,0.316738144166086,
0.319979638214873),.UNSPECIFIED.);
#119=B_SPLINE_CURVE_WITH_KNOTS('',3,(#8385,#8386,#8387,#8388,#8389,#8390,
#8391,#8392,#8393,#8394,#8395,#8396,#8397,#8398,#8399,#8400,#8401,#8402,
#8403,#8404,#8405,#8406,#8407,#8408,#8409,#8410,#8411,#8412,#8413,#8414,
#8415,#8416,#8417,#8418,#8419,#8420,#8421,#8422,#8423,#8424,#8425,#8426,
#8427,#8428,#8429,#8430,#8431,#8432,#8433,#8434,#8435,#8436,#8437,#8438,
#8439,#8440,#8441,#8442,#8443,#8444,#8445,#8446,#8447,#8448,#8449,#8450,
#8451,#8452,#8453,#8454,#8455,#8456,#8457,#8458,#8459,#8460,#8461,#8462,
#8463,#8464,#8465,#8466,#8467,#8468,#8469,#8470,#8471,#8472),
 .UNSPECIFIED.,.F.,.F.,(4,3,3,3,3,3,3,3,3,3,3,3,3,3,3,3,3,3,3,3,3,3,3,3,
3,3,3,3,3,4),(-0.321499574649745,-0.308639510237196,-0.292262552050655,
-0.285372565290688,-0.282077555907296,-0.265037557387853,-0.252192985904029,
-0.24784545954478,-0.243738192672081,-0.226094652565765,-0.208132202142491,
-0.196707016120459,-0.191486671532126,-0.188416440693185,-0.185204704484879,
-0.166696376310579,-0.162287577878747,-0.144403429113291,-0.13537821479371,
-0.129752321066448,-0.125753449476847,-0.107263748186351,-0.0882397721456158,
-0.0692157961048804,-0.0657197649701159,-0.0625694288177743,-0.0429999128835448,
-0.0235085207817788,-0.00419545160864722,0.),.UNSPECIFIED.);
#120=B_SPLINE_CURVE_WITH_KNOTS('',3,(#8473,#8474,#8475,#8476),
 .UNSPECIFIED.,.F.,.F.,(4,4),(0.,0.0112718986101486),.UNSPECIFIED.);
#121=B_SPLINE_CURVE_WITH_KNOTS('',3,(#8477,#8478,#8479,#8480,#8481,#8482,
#8483,#8484,#8485,#8486,#8487,#8488,#8489,#8490,#8491,#8492,#8493,#8494,
#8495,#8496,#8497,#8498,#8499,#8500,#8501,#8502,#8503,#8504,#8505,#8506,
#8507,#8508,#8509,#8510,#8511,#8512,#8513,#8514,#8515,#8516,#8517,#8518,
#8519,#8520,#8521,#8522,#8523,#8524,#8525,#8526,#8527,#8528,#8529,#8530,
#8531,#8532,#8533,#8534,#8535,#8536,#8537,#8538,#8539,#8540,#8541,#8542,
#8543,#8544,#8545,#8546,#8547,#8548,#8549,#8550,#8551,#8552,#8553,#8554,
#8555,#8556,#8557,#8558),.UNSPECIFIED.,.F.,.F.,(4,3,3,3,3,3,3,3,3,3,3,3,
3,3,3,3,3,3,3,3,3,3,3,3,3,3,3,4),(0.,0.0158313618666332,0.0352739749108183,
0.0549065400622293,0.0614660392741775,0.0648988561933009,0.0684243966151204,
0.0875181682202572,0.107484385696968,0.125932139403052,0.127450603173679,
0.130444599968218,0.148719087235956,0.166424962509677,0.176672078090267,
0.186480980745562,0.190515610764009,0.208325400012171,0.226979737992308,
0.244665188163836,0.245634075972445,0.248879896927083,0.266153517834279,
0.280651005930739,0.284205126944081,0.287929482087063,0.304714528368394,
0.321499574649725),.UNSPECIFIED.);
#122=B_SPLINE_CURVE_WITH_KNOTS('',3,(#8676,#8677,#8678,#8679,#8680,#8681,
#8682,#8683),.UNSPECIFIED.,.F.,.F.,(4,1,1,1,1,4),(10.3751771421666,11.3068071567193,
12.3063569665714,13.3059067764236,14.3054565862757,15.1257192387471),
 .UNSPECIFIED.);
#123=B_SPLINE_CURVE_WITH_KNOTS('',3,(#8686,#8687,#8688,#8689,#8690,#8691,
#8692,#8693,#8694,#8695,#8696,#8697,#8698,#8699,#8700,#8701,#8702,#8703,
#8704,#8705,#8706,#8707,#8708,#8709,#8710,#8711,#8712,#8713,#8714,#8715,
#8716,#8717,#8718,#8719,#8720,#8721,#8722,#8723,#8724,#8725,#8726,#8727,
#8728,#8729,#8730,#8731,#8732,#8733,#8734,#8735,#8736,#8737,#8738,#8739,
#8740,#8741,#8742,#8743,#8744,#8745,#8746,#8747,#8748,#8749,#8750,#8751,
#8752,#8753,#8754,#8755,#8756,#8757,#8758,#8759,#8760,#8761,#8762,#8763,
#8764,#8765,#8766,#8767,#8768,#8769,#8770,#8771,#8772,#8773,#8774,#8775,
#8776,#8777,#8778,#8779),.UNSPECIFIED.,.F.,.F.,(4,2,2,2,2,2,2,2,2,2,2,2,
2,2,2,2,2,2,2,2,2,2,2,2,2,2,2,2,2,2,2,2,2,2,2,2,2,2,2,2,2,2,2,2,2,2,4),
(-2.07535699417274,-2.07062624526911,-2.06390397808145,-2.03913496638295,
-2.01054723885914,-1.99466355694519,-1.98597044106963,-1.97810011824729,
-1.96742913432041,-1.93617993541108,-1.90152147750812,-1.89003277159946,
-1.8815263154361,-1.87695834489268,-1.8729734601704,-1.86687528387374,-1.84488951098834,
-1.79878739549274,-1.7862206749192,-1.77883081238585,-1.77203218474349,
-1.76280246808816,-1.73953077312565,-1.70020061595449,-1.68839386433749,
-1.67985016566027,-1.6754535499156,-1.67147820244209,-1.66552760282937,
-1.647152261186,-1.60862847305887,-1.59400947809981,-1.58211143388748,-1.57457733824053,
-1.56734072385867,-1.55670381365091,-1.51422192860002,-1.4878998886173,
-1.48032481757243,-1.47592214047974,-1.47211852010191,-1.46536351188341,
-1.42636243278102,-1.39463510154257,-1.38348036493685,-1.37610595103745,
-1.37340468443901),.UNSPECIFIED.);
#124=B_SPLINE_CURVE_WITH_KNOTS('',3,(#8785,#8786,#8787,#8788,#8789,#8790,
#8791,#8792,#8793,#8794,#8795,#8796,#8797,#8798,#8799,#8800,#8801,#8802,
#8803,#8804,#8805,#8806,#8807,#8808,#8809,#8810,#8811,#8812,#8813,#8814,
#8815,#8816,#8817,#8818,#8819,#8820,#8821,#8822,#8823,#8824,#8825,#8826,
#8827,#8828,#8829,#8830,#8831,#8832,#8833,#8834,#8835,#8836,#8837,#8838,
#8839,#8840,#8841,#8842,#8843,#8844,#8845,#8846,#8847,#8848,#8849,#8850,
#8851,#8852,#8853,#8854,#8855,#8856,#8857,#8858,#8859,#8860,#8861,#8862,
#8863,#8864,#8865,#8866,#8867,#8868,#8869,#8870,#8871,#8872,#8873,#8874,
#8875,#8876,#8877,#8878,#8879,#8880,#8881,#8882,#8883,#8884,#8885,#8886,
#8887,#8888,#8889,#8890,#8891,#8892,#8893,#8894,#8895,#8896,#8897,#8898,
#8899,#8900,#8901,#8902,#8903,#8904,#8905,#8906,#8907,#8908,#8909,#8910,
#8911,#8912,#8913,#8914,#8915,#8916,#8917,#8918,#8919,#8920,#8921,#8922,
#8923,#8924,#8925,#8926,#8927,#8928,#8929,#8930,#8931,#8932,#8933,#8934,
#8935,#8936,#8937,#8938,#8939,#8940,#8941,#8942,#8943,#8944,#8945,#8946,
#8947,#8948,#8949,#8950,#8951,#8952,#8953,#8954,#8955,#8956),
 .UNSPECIFIED.,.F.,.F.,(4,3,3,3,3,3,3,3,3,3,3,3,3,3,3,3,3,3,3,3,3,3,3,3,
3,3,3,3,3,3,3,3,3,3,3,3,3,3,3,3,3,3,3,3,3,3,3,3,3,3,3,3,3,3,3,3,3,4),(15.7079632679489,
15.8140060705019,15.9200901242099,16.0263330305178,16.1326617635271,16.2392097967397,
16.30455620598,16.4094926907624,16.5142711739612,16.6189258395903,16.7235142950206,
16.8280721401984,16.9326349307205,17.0373085987797,17.1420432536121,17.2469612836429,
17.3041060158321,17.4090419624236,17.5138199393734,17.6184741490198,17.7230621798904,
17.8276196326623,17.9321820636969,18.0368554252288,18.1415898031092,18.2465076058582,
18.3036558256843,18.4085885657132,18.5133632718617,18.6180141312869,18.7225987646189,
18.8271527776088,18.931711731645,19.0363815833322,19.141112427443,19.2460266968149,
19.3032056355364,19.4081402098677,19.5129167767403,19.6175695269526,19.7221560686272,
19.8267120046426,19.9312728935312,20.0359446847347,20.1406774739337,20.2455936761873,
20.3027554453886,20.4076898194264,20.5124661874783,20.6171187420747,20.7217050902322,
20.8262608351303,20.9308215356054,21.035493143851,21.1402257529102,21.2451417814176,
21.3023052552407,21.4102199499323),.UNSPECIFIED.);
#125=B_SPLINE_CURVE_WITH_KNOTS('',3,(#8957,#8958,#8959,#8960,#8961),
 .UNSPECIFIED.,.F.,.F.,(4,1,4),(15.1257192387471,15.3050063961278,15.7079567456947),
 .UNSPECIFIED.);
#126=B_SPLINE_CURVE_WITH_KNOTS('',3,(#8962,#8963,#8964,#8965,#8966,#8967,
#8968,#8969,#8970,#8971,#8972,#8973,#8974,#8975,#8976,#8977,#8978,#8979,
#8980,#8981,#8982,#8983,#8984,#8985,#8986,#8987,#8988,#8989,#8990,#8991,
#8992,#8993,#8994,#8995,#8996,#8997,#8998,#8999,#9000,#9001,#9002,#9003,
#9004,#9005,#9006,#9007,#9008,#9009,#9010,#9011,#9012,#9013,#9014,#9015,
#9016,#9017,#9018,#9019,#9020,#9021,#9022,#9023,#9024,#9025,#9026,#9027,
#9028,#9029,#9030,#9031,#9032,#9033,#9034,#9035,#9036,#9037,#9038,#9039,
#9040,#9041,#9042,#9043,#9044,#9045,#9046,#9047,#9048,#9049,#9050,#9051,
#9052,#9053,#9054,#9055,#9056,#9057,#9058,#9059,#9060,#9061,#9062,#9063,
#9064,#9065,#9066,#9067,#9068,#9069,#9070,#9071,#9072,#9073,#9074,#9075,
#9076,#9077,#9078,#9079,#9080,#9081,#9082,#9083,#9084,#9085,#9086,#9087,
#9088,#9089,#9090,#9091,#9092,#9093,#9094,#9095,#9096,#9097,#9098,#9099,
#9100,#9101,#9102,#9103,#9104,#9105,#9106,#9107,#9108,#9109,#9110,#9111,
#9112,#9113,#9114,#9115,#9116,#9117,#9118,#9119,#9120,#9121,#9122,#9123,
#9124,#9125),.UNSPECIFIED.,.F.,.F.,(4,2,2,2,2,2,2,2,2,2,2,2,2,2,2,2,2,2,
2,2,2,2,2,2,2,2,2,2,2,2,2,2,2,2,2,2,2,2,2,2,2,2,2,2,2,2,2,2,2,2,2,2,2,2,
2,2,2,2,2,2,2,2,2,2,2,2,2,2,2,2,2,2,2,2,2,2,2,2,2,2,2,4),(-1.37340468443901,
-1.36871743081555,-1.35748583702605,-1.3200010148775,-1.29672758652404,
-1.28744009490948,-1.28019430521612,-1.27590019966677,-1.2716085688058,
-1.26427445536536,-1.22518572267299,-1.19428746066202,-1.18328761720507,
-1.17599945296877,-1.16869369100309,-1.15759715127668,-1.1181943045483,
-1.09601897457847,-1.0869871962481,-1.07990084592359,-1.07566513746222,
-1.07134135369325,-1.06390168160929,-1.03810159496872,-0.992803412570896,
-0.982338601089973,-0.975177691561462,-0.96770063758569,-0.955857909323519,
-0.941268128320568,-0.902444827390983,-0.884869616820766,-0.878940686944186,
-0.874885335771914,-0.8701287887699,-0.860444431478508,-0.846440319909858,
-0.81679757628812,-0.811538025734025,-0.790068708525572,-0.780999903268975,
-0.773948618441998,-0.765995966563767,-0.751522254455603,-0.731996729298023,
-0.691751235073339,-0.682044394561865,-0.677285813277941,-0.673242944351546,
-0.667351658205613,-0.648687982702851,-0.598586700061476,-0.585406495261867,
-0.577693318198781,-0.570590040383836,-0.560886292698399,-0.531591748652482,
-0.490049087033579,-0.481436396826925,-0.476882546047545,-0.472770001759554,
-0.466425444949794,-0.439660929000518,-0.392740047594552,-0.382512461256994,
-0.375396513289168,-0.367869588254539,-0.355723130340433,-0.322764296660365,
-0.287567482415229,-0.280428805481126,-0.276165142153246,-0.271836165726112,
-0.264372895412004,-0.238768212099689,-0.193299058928824,-0.182872884802073,
-0.175726134313817,-0.168255059270011,-0.156406019240682,-0.141805592911803,
-0.116782820621066),.UNSPECIFIED.);
#127=B_SPLINE_CURVE_WITH_KNOTS('',3,(#9131,#9132,#9133,#9134,#9135,#9136,
#9137,#9138,#9139,#9140,#9141,#9142,#9143,#9144,#9145,#9146,#9147,#9148,
#9149,#9150,#9151,#9152,#9153,#9154,#9155,#9156,#9157,#9158,#9159,#9160,
#9161,#9162,#9163,#9164,#9165,#9166,#9167,#9168,#9169,#9170,#9171,#9172,
#9173,#9174,#9175,#9176,#9177,#9178,#9179,#9180,#9181,#9182,#9183,#9184,
#9185,#9186,#9187,#9188,#9189,#9190,#9191,#9192,#9193,#9194,#9195,#9196,
#9197,#9198,#9199,#9200,#9201,#9202,#9203,#9204,#9205,#9206,#9207,#9208,
#9209,#9210,#9211,#9212,#9213,#9214,#9215,#9216,#9217,#9218,#9219,#9220,
#9221,#9222,#9223,#9224,#9225,#9226,#9227,#9228,#9229,#9230,#9231,#9232,
#9233,#9234,#9235,#9236,#9237,#9238,#9239,#9240,#9241,#9242,#9243,#9244,
#9245,#9246,#9247,#9248,#9249,#9250,#9251,#9252,#9253,#9254,#9255,#9256,
#9257,#9258,#9259,#9260,#9261,#9262,#9263,#9264,#9265,#9266,#9267,#9268,
#9269,#9270,#9271,#9272,#9273,#9274,#9275,#9276,#9277,#9278,#9279,#9280),
 .UNSPECIFIED.,.F.,.F.,(4,2,2,2,2,2,2,2,2,2,2,2,2,2,2,2,2,2,2,2,2,2,2,2,
2,2,2,2,2,2,2,2,2,2,2,2,2,2,2,2,2,2,2,2,2,2,2,2,2,2,2,2,2,2,2,2,2,2,2,2,
2,2,2,2,2,2,2,2,2,2,2,2,2,2,4),(-1.14061870450622,-1.13958195964596,-1.12266879087202,
-1.08281934178168,-1.06959889951782,-1.06471429770308,-1.06068012672009,
-1.05587064594565,-1.04587632392007,-0.999418617025877,-0.976433036897593,
-0.967166228933324,-0.960092877789842,-0.952248888383839,-0.938376963922012,
-0.920052937498073,-0.894060657937701,-0.871556239654625,-0.865322258102495,
-0.861267461095725,-0.856682550344552,-0.847919948238388,-0.801100630640885,
-0.799115970822433,-0.776456064607275,-0.767226345807944,-0.76015819165588,
-0.752296729049045,-0.738324922715054,-0.719803447177033,-0.693815912555669,
-0.67165232509663,-0.665434233695802,-0.661382280499621,-0.656791660709034,
-0.64799739350855,-0.606818368303741,-0.577680011860102,-0.567920265960079,
-0.560804794226708,-0.553104033972044,-0.540012435378701,-0.516652027872025,
-0.473266797217643,-0.466300249493322,-0.462071551381904,-0.457702709275398,
-0.450041696240669,-0.440005173513315,-0.412835238526543,-0.380872948511376,
-0.369743491624624,-0.362402893987223,-0.35506506155264,-0.343951299162992,
-0.312385485717975,-0.272863502890842,-0.266179132741583,-0.26241555881735,
-0.258115242971251,-0.250793298578873,-0.226411012152923,-0.17878218694598,
-0.168659285477799,-0.161560276461644,-0.154003631587863,-0.14169344121923,
-0.11377328835674,-0.0754140544872524,-0.0673951691566298,-0.0629547708213861,
-0.0587770332817225,-0.0520752430550884,-0.0212767115436388,-0.000594353055929244),
 .UNSPECIFIED.);
#128=B_SPLINE_CURVE_WITH_KNOTS('',3,(#9281,#9282,#9283,#9284,#9285,#9286,
#9287,#9288,#9289,#9290,#9291,#9292,#9293,#9294,#9295,#9296,#9297,#9298,
#9299),.UNSPECIFIED.,.F.,.F.,(4,3,3,3,3,3,4),(21.4102199499323,21.5145277033485,
21.6187228794953,21.722854083458,21.8269466273695,21.9310741676971,21.9911485751285),
 .UNSPECIFIED.);
#129=B_SPLINE_CURVE_WITH_KNOTS('',3,(#9301,#9302,#9303,#9304,#9305,#9306,
#9307,#9308,#9309,#9310,#9311,#9312,#9313,#9314,#9315,#9316,#9317,#9318),
 .UNSPECIFIED.,.F.,.F.,(4,2,2,2,2,2,2,2,4),(-0.116782820621066,-0.102980098125634,
-0.085284604519627,-0.0793273984135347,-0.0752749720407285,-0.0705497398843767,
-0.06102445685247,-0.0473538417127571,-0.00061658398721623),
 .UNSPECIFIED.);
#130=B_SPLINE_CURVE_WITH_KNOTS('',3,(#9319,#9320,#9321,#9322,#9323,#9324,
#9325,#9326,#9327,#9328,#9329,#9330,#9331,#9332,#9333,#9334,#9335,#9336,
#9337,#9338,#9339,#9340,#9341,#9342,#9343,#9344,#9345,#9346,#9347,#9348,
#9349,#9350,#9351,#9352,#9353,#9354,#9355,#9356,#9357,#9358,#9359,#9360,
#9361,#9362,#9363,#9364,#9365,#9366,#9367,#9368,#9369,#9370,#9371,#9372,
#9373,#9374,#9375,#9376,#9377,#9378,#9379,#9380,#9381,#9382,#9383,#9384,
#9385,#9386,#9387,#9388,#9389,#9390,#9391,#9392,#9393,#9394,#9395,#9396,
#9397,#9398,#9399,#9400,#9401,#9402,#9403,#9404,#9405,#9406,#9407,#9408,
#9409,#9410,#9411,#9412,#9413,#9414,#9415,#9416,#9417,#9418,#9419,#9420,
#9421,#9422,#9423,#9424,#9425,#9426,#9427,#9428,#9429,#9430,#9431,#9432,
#9433,#9434,#9435,#9436,#9437,#9438,#9439,#9440,#9441,#9442,#9443,#9444,
#9445,#9446,#9447,#9448,#9449,#9450,#9451,#9452,#9453,#9454,#9455,#9456,
#9457,#9458,#9459,#9460,#9461,#9462,#9463,#9464,#9465,#9466,#9467,#9468,
#9469,#9470,#9471,#9472,#9473,#9474),.UNSPECIFIED.,.F.,.F.,(4,2,2,2,2,2,
2,2,2,2,2,2,2,2,2,2,2,2,2,2,2,2,2,2,2,2,2,2,2,2,2,2,2,2,2,2,2,2,2,2,2,2,
2,2,2,2,2,2,2,2,2,2,2,2,2,2,2,2,2,2,2,2,2,2,2,2,2,2,2,2,2,2,2,2,2,2,2,4),
(-2.51378437080705,-2.50403412993197,-2.49569275978735,-2.4890492244808,
-2.48247746651656,-2.47156832709352,-2.43112912652391,-2.40958993904581,
-2.40069266360761,-2.39367754444654,-2.38944008648743,-2.3850849117104,
-2.37748874337329,-2.33868487780727,-2.31048225053466,-2.29818897115585,
-2.29063663288652,-2.28353790617523,-2.27340912602132,-2.22578723704126,
-2.20137359621892,-2.19404819352388,-2.18974775666784,-2.18598580437682,
-2.17930772677495,-2.13976604713605,-2.10823733424573,-2.09712971628745,
-2.08979408129866,-2.08245438588889,-2.07132424549092,-2.03256101584112,
-2.01019268342857,-2.00111140656932,-1.99398988861816,-1.98973091019721,
-1.98593957491622,-1.97909176364722,-1.94107284853398,-1.90860126763712,
-1.89737409170347,-1.89001717454648,-1.88269853975448,-1.87168596483596,
-1.84317218534402,-1.81858185768069,-1.80513781418202,-1.79572151108212,
-1.79101608653026,-1.78695823582036,-1.78096166148747,-1.76211273249074,
-1.72427362390954,-1.70982229066988,-1.69805894240342,-1.69060420516893,
-1.68344794478296,-1.67296076088694,-1.62790910643968,-1.60882407495956,
-1.59698695384212,-1.59187884999028,-1.587881968817,-1.58259968637489,-1.57049888342963,
-1.52613809762451,-1.51084393113901,-1.49859846821437,-1.49105467975322,
-1.48395094353315,-1.47379181203992,-1.42636992345633,-1.40184009580425,
-1.39450071182093,-1.39019731016868,-1.38591207155117,-1.37866220630911,
-1.37342554502812),.UNSPECIFIED.);
#131=B_SPLINE_CURVE_WITH_KNOTS('',3,(#9479,#9480,#9481,#9482,#9483,#9484,
#9485,#9486,#9487,#9488,#9489,#9490,#9491,#9492,#9493,#9494,#9495,#9496,
#9497,#9498,#9499,#9500,#9501,#9502,#9503,#9504,#9505,#9506,#9507,#9508,
#9509,#9510,#9511,#9512,#9513,#9514,#9515,#9516,#9517,#9518,#9519,#9520,
#9521,#9522,#9523,#9524,#9525,#9526,#9527,#9528,#9529,#9530,#9531,#9532,
#9533,#9534,#9535,#9536,#9537,#9538,#9539,#9540,#9541,#9542,#9543,#9544,
#9545,#9546,#9547,#9548,#9549,#9550,#9551,#9552,#9553,#9554,#9555,#9556,
#9557,#9558,#9559,#9560,#9561,#9562,#9563,#9564,#9565,#9566,#9567,#9568,
#9569,#9570,#9571,#9572,#9573,#9574,#9575,#9576,#9577,#9578,#9579,#9580,
#9581,#9582,#9583,#9584,#9585,#9586,#9587,#9588,#9589,#9590,#9591,#9592,
#9593,#9594,#9595,#9596,#9597,#9598,#9599,#9600,#9601,#9602,#9603,#9604,
#9605,#9606,#9607,#9608,#9609,#9610,#9611,#9612,#9613,#9614,#9615,#9616,
#9617,#9618,#9619,#9620,#9621,#9622,#9623,#9624,#9625,#9626,#9627,#9628,
#9629,#9630,#9631,#9632,#9633,#9634,#9635,#9636,#9637,#9638,#9639,#9640),
 .UNSPECIFIED.,.F.,.F.,(4,2,2,2,2,2,2,2,2,2,2,2,2,2,2,2,2,2,2,2,2,2,2,2,
2,2,2,2,2,2,2,2,2,2,2,2,2,2,2,2,2,2,2,2,2,2,2,2,2,2,2,2,2,2,2,2,2,2,2,2,
2,2,2,2,2,2,2,2,2,2,2,2,2,2,2,2,2,2,2,2,4),(-2.39712982154602,-2.37982822062964,
-2.36865519395186,-2.36130697773033,-2.35397711103529,-2.34290705949758,
-2.30322269035014,-2.27203351873412,-2.26519392855631,-2.26099006907781,
-2.25658860397391,-2.24876473218744,-2.21021735720178,-2.18219173395406,
-2.16988518348984,-2.16232945507946,-2.15523034487358,-2.14670714630564,
-2.12298763570221,-2.07728526027882,-2.06741562350919,-2.06262840655135,
-2.05859008504526,-2.0527460756908,-2.03595372179219,-1.99628036112784,
-1.98156521764677,-1.96964904440506,-1.96216489337884,-1.95502446924087,
-1.94464244695748,-1.89880747281565,-1.87263665982996,-1.86560192359237,
-1.86135942682898,-1.85700648900914,-1.84942584938645,-1.81961990294089,
-1.79172799479035,-1.77912062417306,-1.76845651929048,-1.76119687894259,
-1.75463962397716,-1.74383518181111,-1.70132948089653,-1.67273853853663,
-1.66571201038827,-1.66147104391196,-1.6571159371628,-1.6495250466247,-1.62096258023062,
-1.58187612035999,-1.56990812464652,-1.56241413754037,-1.55527909917317,
-1.54493220248383,-1.49883577875733,-1.47356474731669,-1.46613856692982,
-1.46181676485615,-1.45754638164616,-1.45037367011324,-1.41575255653518,
-1.38212339666726,-1.3700711994623,-1.36256139372232,-1.35543508155993,
-1.34514442048775,-1.29863746327514,-1.27216652507063,-1.26552237131373,
-1.26135498595559,-1.25689625480186,-1.24878711935642,-1.23792668529515,
-1.20577170339601,-1.17728442476895,-1.16754158552402,-1.16042715070981,
-1.1527171437714,-1.14061870450622),.UNSPECIFIED.);
#132=B_SPLINE_CURVE_WITH_KNOTS('',3,(#9641,#9642,#9643,#9644,#9645,#9646,
#9647,#9648,#9649,#9650,#9651,#9652,#9653,#9654,#9655,#9656,#9657,#9658,
#9659,#9660,#9661,#9662,#9663,#9664,#9665,#9666,#9667,#9668,#9669,#9670,
#9671,#9672,#9673,#9674,#9675,#9676,#9677,#9678,#9679,#9680,#9681,#9682,
#9683,#9684,#9685,#9686,#9687,#9688,#9689,#9690,#9691,#9692,#9693,#9694,
#9695,#9696,#9697,#9698,#9699,#9700,#9701,#9702,#9703,#9704,#9705,#9706,
#9707,#9708,#9709,#9710,#9711,#9712,#9713,#9714,#9715,#9716,#9717,#9718,
#9719,#9720,#9721,#9722,#9723,#9724,#9725,#9726,#9727,#9728,#9729,#9730,
#9731,#9732,#9733,#9734,#9735,#9736,#9737,#9738,#9739,#9740,#9741,#9742,
#9743,#9744,#9745,#9746,#9747,#9748,#9749,#9750,#9751,#9752,#9753,#9754,
#9755,#9756,#9757,#9758,#9759,#9760,#9761,#9762,#9763,#9764,#9765,#9766,
#9767,#9768,#9769,#9770,#9771,#9772,#9773,#9774,#9775,#9776,#9777,#9778,
#9779,#9780,#9781,#9782,#9783,#9784,#9785,#9786,#9787,#9788,#9789,#9790,
#9791,#9792,#9793,#9794,#9795,#9796,#9797,#9798),.UNSPECIFIED.,.F.,.F.,
(4,2,2,2,2,2,2,2,2,2,2,2,2,2,2,2,2,2,2,2,2,2,2,2,2,2,2,2,2,2,2,2,2,2,2,
2,2,2,2,2,2,2,2,2,2,2,2,2,2,2,2,2,2,2,2,2,2,2,2,2,2,2,2,2,2,2,2,2,2,2,2,
2,2,2,2,2,2,2,4),(-1.37342554502812,-1.33696888519612,-1.31599588280204,
-1.30083372389245,-1.29276344707354,-1.28573464590891,-1.27671691634361,
-1.25701206626934,-1.22203976080302,-1.19977452572423,-1.1935519713523,
-1.18949971434911,-1.18491216460396,-1.17613234532156,-1.13518072828273,
-1.1057937615912,-1.09602774370631,-1.08891214603407,-1.08121550618681,
-1.06814289170902,-1.04441797874472,-1.00150686267968,-0.994457653340163,
-0.990212921266357,-0.985865078057203,-0.978306536753042,-0.951838422854677,
-0.907830865572262,-0.897213297876052,-0.890035291338718,-0.882611335137387,
-0.87101663977932,-0.856853444677602,-0.820884985122024,-0.799863535275151,
-0.793695479516006,-0.789651979329424,-0.785042309942625,-0.776144499491377,
-0.763758746982642,-0.718618715741055,-0.701985338797066,-0.693670919387845,
-0.686730787430037,-0.678081381148968,-0.659236756575006,-0.6288700647275,
-0.602489099950622,-0.595034534733468,-0.590708088271243,-0.586445484469463,
-0.579305810914881,-0.570193882432757,-0.547679508863399,-0.50920321758957,
-0.498061865773953,-0.490720365046891,-0.483386956059274,-0.472291126056974,
-0.440856639292396,-0.401114053743307,-0.394454688556459,-0.390695988214397,
-0.386390841739503,-0.379042034747994,-0.354426112834819,-0.307214774795675,
-0.29703259743498,-0.289925694224372,-0.282389439735313,-0.270182987341686,
-0.23694231788426,-0.202182775892267,-0.195016484547438,-0.190748523634948,
-0.186427790448431,-0.179001931413061,-0.153718969852119,-0.116908344231473),
 .UNSPECIFIED.);
#133=B_SPLINE_CURVE_WITH_KNOTS('',3,(#9804,#9805,#9806,#9807,#9808,#9809,
#9810,#9811,#9812,#9813,#9814,#9815,#9816,#9817,#9818,#9819,#9820,#9821,
#9822,#9823,#9824,#9825,#9826,#9827,#9828,#9829,#9830,#9831,#9832,#9833,
#9834,#9835,#9836,#9837,#9838,#9839,#9840,#9841,#9842,#9843,#9844,#9845,
#9846,#9847,#9848,#9849,#9850,#9851,#9852,#9853,#9854,#9855,#9856,#9857,
#9858,#9859,#9860,#9861,#9862,#9863,#9864,#9865,#9866,#9867,#9868,#9869,
#9870,#9871,#9872,#9873,#9874,#9875,#9876,#9877,#9878,#9879,#9880,#9881,
#9882,#9883,#9884,#9885,#9886,#9887,#9888,#9889,#9890,#9891,#9892,#9893,
#9894,#9895,#9896,#9897,#9898,#9899,#9900,#9901,#9902,#9903,#9904,#9905,
#9906,#9907,#9908,#9909,#9910,#9911,#9912,#9913,#9914,#9915,#9916,#9917,
#9918,#9919,#9920,#9921,#9922,#9923,#9924,#9925,#9926,#9927,#9928,#9929,
#9930,#9931,#9932,#9933,#9934,#9935,#9936,#9937,#9938,#9939,#9940,#9941,
#9942,#9943,#9944,#9945,#9946,#9947,#9948,#9949,#9950,#9951),
 .UNSPECIFIED.,.F.,.F.,(4,2,2,2,2,2,2,2,2,2,2,2,2,2,2,2,2,2,2,2,2,2,2,2,
2,2,2,2,2,2,2,2,2,2,2,2,2,2,2,2,2,2,2,2,2,2,2,2,2,2,2,2,2,2,2,2,2,2,2,2,
2,2,2,2,2,2,2,2,2,2,2,2,2,4),(-1.14097344694939,-1.13646400189371,-1.1272692673211,
-1.1043715879283,-1.06651269588549,-1.05534360370122,-1.04799598085995,
-1.04066523591785,-1.02959087664762,-0.998328570863161,-0.958311683721402,
-0.951683248647658,-0.947929237353639,-0.943614324414954,-0.936220341227765,
-0.911220910509429,-0.864704478268882,-0.854424034243729,-0.847300413186092,
-0.839789699374971,-0.827727506389926,-0.789091707982635,-0.760268461203665,
-0.752654206773099,-0.748294784768412,-0.744058328519856,-0.737053065241778,
-0.728174494290414,-0.706717110443944,-0.666442340431915,-0.655422435981745,
-0.648101226052769,-0.640743153429538,-0.629517000033496,-0.597067149632733,
-0.558970652836188,-0.552126791864149,-0.548335482489455,-0.544073736764986,
-0.536942388819262,-0.527845649679413,-0.505404300443613,-0.466810230385369,
-0.455673460605494,-0.448331200953813,-0.440994047856292,-0.429886085925357,
-0.398368874800689,-0.358761651094981,-0.352086110115651,-0.348323877618132,
-0.344020907956559,-0.336686766343578,-0.312203528815908,-0.264752030232991,
-0.25460260043251,-0.247499144062276,-0.239949846260566,-0.227681159287737,
-0.212344962657144,-0.167646029963723,-0.155815887049593,-0.150575733395198,
-0.146579338644274,-0.141429728618438,-0.129319280740467,-0.109510257460682,
-0.0659694565309138,-0.0553200026572353,-0.0481352911225703,-0.0407159436544367,
-0.0331545468549584,-0.0213394885155918,-0.000593737719980223),
 .UNSPECIFIED.);
#134=B_SPLINE_CURVE_WITH_KNOTS('',3,(#9952,#9953,#9954,#9955,#9956,#9957,
#9958,#9959,#9960,#9961,#9962,#9963,#9964,#9965,#9966,#9967),
 .UNSPECIFIED.,.F.,.F.,(4,2,2,2,2,2,2,4),(-2.51321608836282,-2.47261480947244,
-2.46539989016161,-2.46112157445569,-2.4573432595597,-2.45057262653564,
-2.41186419033852,-2.39712982154602),.UNSPECIFIED.);
#135=B_SPLINE_CURVE_WITH_KNOTS('',3,(#9969,#9970,#9971,#9972,#9973,#9974,
#9975,#9976,#9977,#9978,#9979,#9980,#9981,#9982,#9983,#9984,#9985,#9986),
 .UNSPECIFIED.,.F.,.F.,(4,2,2,2,2,2,2,2,4),(-0.116908344231473,-0.107697949475263,
-0.0973491581199381,-0.0902159090932756,-0.0827264498688542,-0.0707726724833073,
-0.031819298716922,-0.00902562018967192,-0.000594336423203717),
 .UNSPECIFIED.);
#136=B_SPLINE_CURVE_WITH_KNOTS('',3,(#9987,#9988,#9989,#9990,#9991,#9992,
#9993,#9994,#9995,#9996,#9997,#9998,#9999,#10000,#10001,#10002,#10003,#10004,
#10005,#10006,#10007,#10008,#10009,#10010,#10011,#10012,#10013,#10014,#10015,
#10016,#10017,#10018,#10019,#10020,#10021,#10022,#10023,#10024,#10025,#10026,
#10027,#10028,#10029,#10030,#10031,#10032,#10033,#10034,#10035,#10036,#10037,
#10038,#10039,#10040,#10041,#10042,#10043,#10044,#10045,#10046,#10047,#10048,
#10049,#10050,#10051,#10052,#10053,#10054,#10055,#10056,#10057,#10058,#10059,
#10060,#10061,#10062,#10063,#10064,#10065,#10066,#10067,#10068,#10069,#10070,
#10071,#10072,#10073,#10074,#10075,#10076,#10077,#10078,#10079,#10080,#10081,
#10082,#10083,#10084,#10085,#10086,#10087,#10088,#10089,#10090,#10091,#10092,
#10093,#10094,#10095,#10096,#10097,#10098,#10099,#10100,#10101,#10102,#10103,
#10104,#10105,#10106,#10107,#10108,#10109,#10110,#10111,#10112,#10113,#10114,
#10115,#10116,#10117,#10118,#10119,#10120,#10121,#10122,#10123,#10124,#10125,
#10126,#10127,#10128,#10129,#10130,#10131,#10132,#10133,#10134,#10135,#10136,
#10137,#10138,#10139,#10140,#10141,#10142),.UNSPECIFIED.,.F.,.F.,(4,2,2,
2,2,2,2,2,2,2,2,2,2,2,2,2,2,2,2,2,2,2,2,2,2,2,2,2,2,2,2,2,2,2,2,2,2,2,2,
2,2,2,2,2,2,2,2,2,2,2,2,2,2,2,2,2,2,2,2,2,2,2,2,2,2,2,2,2,2,2,2,2,2,2,2,
2,2,4),(-2.5139771603986,-2.50974231440594,-2.50550766132944,-2.50154507535624,
-2.4957462142949,-2.47922982302599,-2.46210389994978,-2.4378966219083,-2.41752514377281,
-2.40866940415638,-2.40165396777123,-2.39347579910472,-2.37816882780702,
-2.33145804647038,-2.31893107799337,-2.30996346440651,-2.30534090013258,
-2.30130241623188,-2.29516578641853,-2.27612107492151,-2.2386601327274,
-2.22426612998011,-2.21253617441478,-2.20508777725738,-2.19792771607934,
-2.18741623335324,-2.14255199934756,-2.12338213763505,-2.1115128093502,
-2.10639998108809,-2.10240348350174,-2.09712692763231,-2.08506222428278,
-2.04066251390605,-2.02536444500856,-2.01311691278679,-2.00557293655083,
-1.99846970636383,-1.98831251685999,-1.94088154276745,-1.91635867308484,
-1.9090202716227,-1.90471717167386,-1.90095686331538,-1.89428889175171,
-1.85465251314199,-1.82317896996235,-1.81207813779998,-1.80474346917739,
-1.79740212821455,-1.78626414060057,-1.7476352919286,-1.72518328287483,
-1.71608359358885,-1.70895139795921,-1.70469012944518,-1.70090018578456,
-1.69406109583143,-1.65595905273851,-1.62353671474701,-1.61231531633278,
-1.60495913940849,-1.59763900645014,-1.58661967163277,-1.55799067849915,
-1.51927059611237,-1.51035098109844,-1.50573702499238,-1.50169468115358,
-1.49553567122442,-1.4746620051643,-1.43859743071974,-1.42442109879224,
-1.41281752020196,-1.40539154504965,-1.39821395422413,-1.38760175305837,
-1.37383024056511),.UNSPECIFIED.);
#137=B_SPLINE_CURVE_WITH_KNOTS('',3,(#10147,#10148,#10149,#10150,#10151,
#10152,#10153,#10154,#10155,#10156,#10157,#10158,#10159,#10160,#10161,#10162,
#10163,#10164,#10165,#10166,#10167,#10168,#10169,#10170,#10171,#10172,#10173,
#10174,#10175,#10176,#10177,#10178,#10179,#10180,#10181,#10182,#10183,#10184,
#10185,#10186,#10187,#10188,#10189,#10190,#10191,#10192,#10193,#10194,#10195,
#10196,#10197,#10198,#10199,#10200,#10201,#10202,#10203,#10204,#10205,#10206,
#10207,#10208,#10209,#10210,#10211,#10212,#10213,#10214,#10215,#10216,#10217,
#10218,#10219,#10220,#10221,#10222,#10223,#10224,#10225,#10226,#10227,#10228,
#10229,#10230,#10231,#10232,#10233,#10234,#10235,#10236,#10237,#10238,#10239,
#10240,#10241,#10242,#10243,#10244,#10245,#10246,#10247,#10248,#10249,#10250,
#10251,#10252,#10253,#10254,#10255,#10256,#10257,#10258,#10259,#10260,#10261,
#10262,#10263,#10264,#10265,#10266,#10267,#10268,#10269,#10270,#10271,#10272,
#10273,#10274,#10275,#10276,#10277,#10278,#10279,#10280,#10281,#10282,#10283,
#10284,#10285,#10286,#10287,#10288,#10289,#10290,#10291,#10292,#10293,#10294,
#10295,#10296,#10297,#10298,#10299,#10300,#10301,#10302,#10303,#10304,#10305,
#10306,#10307,#10308,#10309,#10310,#10311,#10312,#10313,#10314,#10315,#10316),
 .UNSPECIFIED.,.F.,.F.,(4,2,2,2,2,2,2,2,2,2,2,2,2,2,2,2,2,2,2,2,2,2,2,2,
2,2,2,2,2,2,2,2,2,2,2,2,2,2,2,2,2,2,2,2,2,2,2,2,2,2,2,2,2,2,2,2,2,2,2,2,
2,2,2,2,2,2,2,2,2,2,2,2,2,2,2,2,2,2,2,2,2,2,2,2,4),(-2.39716550844473,-2.38235738603314,
-2.35842144763977,-2.35115384039938,-2.34686562342799,-2.34309596376143,
-2.33637218037512,-2.29726343256587,-2.26548629893112,-2.25434752545061,
-2.24700638275891,-2.23967212728965,-2.22857211700272,-2.1893637225085,
-2.16728042196396,-2.15826235349736,-2.15117742777478,-2.14692578197953,
-2.14258647615187,-2.13506865455545,-2.1072780138158,-2.07799254417099,
-2.0595097647271,-2.05091277446615,-2.04390797212759,-2.03551737455716,
-2.01840446400436,-1.97387414855571,-1.96154105035962,-1.95267052327612,
-1.94806600128552,-1.94402035125614,-1.93783907130222,-1.91655293707972,
-1.88084868021968,-1.86673290115953,-1.85516521884818,-1.84774611346243,
-1.84056401947354,-1.8299232640557,-1.78607780077785,-1.75949692691008,
-1.75192595740346,-1.74757557620068,-1.74333243335886,-1.73629206997448,
-1.70005579598112,-1.66790033187141,-1.65580608857251,-1.6482898184602,
-1.64117000733272,-1.6309117220091,-1.58420419681792,-1.55928860303882,
-1.55190419999156,-1.54759141965172,-1.54383639354996,-1.53720131043032,
-1.49728191798483,-1.46599148056203,-1.45491417802411,-1.44758305789801,
-1.44023613280808,-1.42907052557603,-1.39104762333584,-1.3682266188749,
-1.35904734943522,-1.35186941780441,-1.3475986186538,-1.34327910839688,
-1.33586165488846,-1.31086987103338,-1.28838349155678,-1.27076716258182,
-1.25726023587208,-1.24948334515615,-1.2423928378255,-1.23281805248766,
-1.20541977550243,-1.18421102044453,-1.15964926327666,-1.15224172666494,
-1.14792424228513,-1.14365142107152,-1.14097344694939),.UNSPECIFIED.);
#138=B_SPLINE_CURVE_WITH_KNOTS('',3,(#10317,#10318,#10319,#10320,#10321,
#10322,#10323,#10324,#10325,#10326,#10327,#10328,#10329,#10330,#10331,#10332,
#10333,#10334,#10335,#10336,#10337,#10338,#10339,#10340,#10341,#10342,#10343,
#10344,#10345,#10346,#10347,#10348,#10349,#10350,#10351,#10352,#10353,#10354,
#10355,#10356,#10357,#10358,#10359,#10360,#10361,#10362,#10363,#10364,#10365,
#10366,#10367,#10368,#10369,#10370,#10371,#10372,#10373,#10374,#10375,#10376,
#10377,#10378,#10379,#10380,#10381,#10382,#10383,#10384,#10385,#10386,#10387,
#10388,#10389,#10390,#10391,#10392,#10393,#10394,#10395,#10396,#10397,#10398,
#10399,#10400,#10401,#10402,#10403,#10404,#10405,#10406,#10407,#10408,#10409,
#10410,#10411,#10412,#10413,#10414,#10415,#10416,#10417,#10418,#10419,#10420,
#10421,#10422,#10423,#10424,#10425,#10426,#10427,#10428,#10429,#10430,#10431,
#10432,#10433,#10434,#10435,#10436,#10437,#10438,#10439,#10440,#10441,#10442,
#10443,#10444,#10445,#10446,#10447,#10448,#10449,#10450,#10451,#10452,#10453,
#10454,#10455,#10456,#10457,#10458,#10459,#10460,#10461,#10462,#10463,#10464,
#10465,#10466,#10467,#10468,#10469,#10470),.UNSPECIFIED.,.F.,.F.,(4,2,2,
2,2,2,2,2,2,2,2,2,2,2,2,2,2,2,2,2,2,2,2,2,2,2,2,2,2,2,2,2,2,2,2,2,2,2,2,
2,2,2,2,2,2,2,2,2,2,2,2,2,2,2,2,2,2,2,2,2,2,2,2,2,2,2,2,2,2,2,2,2,2,2,2,
2,4),(-1.37383024056511,-1.34349731540928,-1.31705490309835,-1.30949832522974,
-1.30515066541329,-1.30090502287577,-1.29385286769016,-1.25770689987854,
-1.22362942230147,-1.21245255606101,-1.20510365224169,-1.19777464244973,
-1.18670939150684,-1.15552063823869,-1.1153573229877,-1.10874342925435,
-1.10499193043474,-1.1006734934197,-1.0932619850194,-1.0681130421046,-1.02183621388935,
-1.01151920481442,-1.00438987030478,-0.996889617840733,-0.984883613661946,
-0.950076256323802,-0.916575705536087,-0.909357259131994,-0.905078194646556,
-0.900767563171138,-0.89339419901032,-0.868574597606939,-0.821713846778265,
-0.811479042593566,-0.804362906709166,-0.796840019979762,-0.784710873386791,
-0.75052981776179,-0.716604504437372,-0.709406180853282,-0.705131254463527,
-0.700816455480394,-0.693422243709192,-0.668421793835061,-0.621885837497626,
-0.611605740278395,-0.604482552356341,-0.596972639663292,-0.584913027143422,
-0.552379595811848,-0.5164487560532,-0.509371911653121,-0.505121479831962,
-0.500779692074401,-0.493252029552087,-0.467068232997983,-0.422580701263669,
-0.412023526501566,-0.40485525773917,-0.397416579128286,-0.385743377964248,
-0.371446062606456,-0.334640239415005,-0.331167944570213,-0.314092075074438,
-0.308223006489398,-0.304182164814755,-0.299410325417555,-0.289625381471665,
-0.275402922450765,-0.226794148326838,-0.214175233539595,-0.206562449046453,
-0.199412490105201,-0.189412365137428,-0.153042973105517,-0.117060520499069),
 .UNSPECIFIED.);
#139=B_SPLINE_CURVE_WITH_KNOTS('',3,(#10476,#10477,#10478,#10479,#10480,
#10481,#10482,#10483,#10484,#10485,#10486,#10487,#10488,#10489,#10490,#10491,
#10492,#10493,#10494,#10495,#10496,#10497,#10498,#10499,#10500,#10501,#10502,
#10503,#10504,#10505,#10506,#10507,#10508,#10509,#10510,#10511,#10512,#10513,
#10514,#10515,#10516,#10517,#10518,#10519,#10520,#10521,#10522,#10523,#10524,
#10525,#10526,#10527,#10528,#10529,#10530,#10531,#10532,#10533,#10534,#10535,
#10536,#10537,#10538,#10539,#10540,#10541,#10542,#10543,#10544,#10545,#10546,
#10547,#10548,#10549,#10550,#10551,#10552,#10553,#10554,#10555,#10556,#10557,
#10558,#10559,#10560,#10561,#10562,#10563,#10564,#10565,#10566,#10567,#10568,
#10569,#10570,#10571,#10572,#10573,#10574,#10575,#10576,#10577,#10578,#10579,
#10580,#10581,#10582,#10583,#10584,#10585,#10586,#10587,#10588,#10589,#10590,
#10591,#10592,#10593,#10594,#10595,#10596,#10597,#10598,#10599,#10600,#10601,
#10602,#10603,#10604,#10605,#10606,#10607,#10608,#10609,#10610,#10611,#10612,
#10613,#10614,#10615,#10616,#10617,#10618,#10619,#10620,#10621,#10622,#10623,
#10624,#10625),.UNSPECIFIED.,.F.,.F.,(4,2,2,2,2,2,2,2,2,2,2,2,2,2,2,2,2,
2,2,2,2,2,2,2,2,2,2,2,2,2,2,2,2,2,2,2,2,2,2,2,2,2,2,2,2,2,2,2,2,2,2,2,2,
2,2,2,2,2,2,2,2,2,2,2,2,2,2,2,2,2,2,2,2,2,4),(-1.14066834730415,-1.13528708228451,
-1.12825874370977,-1.11908952757347,-1.09679743353057,-1.09405211095703,
-1.05799686607207,-1.04142723336169,-1.03574582603282,-1.03173946765447,
-1.02688599334257,-1.0166347101821,-1.0013895134999,-0.949578516067516,
-0.939351418593466,-0.932227839927205,-0.924684865519697,-0.91248856322471,
-0.88103571118122,-0.84434028124934,-0.837351590564754,-0.833111747206177,
-0.82873653939268,-0.82105720118224,-0.810989956120682,-0.783660025081896,
-0.751928535848876,-0.740804028318319,-0.733461603689559,-0.726117783786739,
-0.714985993738198,-0.68330721460369,-0.643929042402749,-0.637224870169614,
-0.633457623199097,-0.629164660474318,-0.621871921607312,-0.597722363135909,
-0.549663362388753,-0.539605197993634,-0.532448911988693,-0.524860290457296,
-0.51236008205074,-0.482998575266667,-0.444104625300159,-0.437349581753881,
-0.433575455096387,-0.429294418534457,-0.422067567339357,-0.391068271416759,
-0.352049912296781,-0.340936279149132,-0.333597222338206,-0.326254155837573,
-0.315118121898445,-0.283383210420531,-0.244161853391143,-0.237444692321296,
-0.233674632362936,-0.229381206936217,-0.222094795011784,-0.198014624474899,
-0.149831759319823,-0.139788442362888,-0.132630526681158,-0.125029029589257,
-0.112478218150378,-0.0827830876071397,-0.0450813175921124,-0.0379343399491491,
-0.0336695761806261,-0.0293431468026109,-0.0247229939503656,-0.0162435752141435,
-0.000615599677778074),.UNSPECIFIED.);
#140=B_SPLINE_CURVE_WITH_KNOTS('',3,(#10626,#10627,#10628,#10629,#10630,
#10631,#10632,#10633,#10634,#10635,#10636,#10637,#10638,#10639),
 .UNSPECIFIED.,.F.,.F.,(4,2,2,2,2,2,4),(-2.51359551756059,-2.46820697681293,
-2.45559533539021,-2.44798484919415,-2.44083562026429,-2.43083389655103,
-2.39716550844473),.UNSPECIFIED.);
#141=B_SPLINE_CURVE_WITH_KNOTS('',3,(#10641,#10642,#10643,#10644,#10645,
#10646,#10647,#10648,#10649,#10650,#10651,#10652,#10653,#10654,#10655,#10656,
#10657,#10658,#10659,#10660,#10661,#10662),.UNSPECIFIED.,.F.,.F.,(4,2,2,
2,2,2,2,2,2,2,4),(-0.117060520499069,-0.116506876729,-0.109491812339823,
-0.105253945341782,-0.100898190861845,-0.0932999678296215,-0.0664641804689692,
-0.0235325687190956,-0.0128214917675811,-0.0060588672363243,-0.000775673896845518),
 .UNSPECIFIED.);
#142=B_SPLINE_CURVE_WITH_KNOTS('',3,(#10663,#10664,#10665,#10666,#10667,
#10668,#10669,#10670,#10671,#10672,#10673,#10674,#10675,#10676,#10677,#10678,
#10679,#10680,#10681,#10682,#10683,#10684,#10685,#10686,#10687,#10688,#10689,
#10690,#10691,#10692,#10693,#10694,#10695,#10696,#10697,#10698,#10699,#10700,
#10701,#10702,#10703,#10704,#10705,#10706,#10707,#10708,#10709,#10710,#10711,
#10712,#10713,#10714,#10715,#10716,#10717,#10718,#10719,#10720,#10721,#10722,
#10723,#10724,#10725,#10726,#10727,#10728,#10729,#10730,#10731,#10732,#10733,
#10734,#10735,#10736,#10737,#10738,#10739,#10740,#10741,#10742,#10743,#10744,
#10745,#10746,#10747,#10748,#10749,#10750,#10751,#10752,#10753,#10754,#10755,
#10756,#10757,#10758,#10759,#10760,#10761,#10762,#10763,#10764,#10765,#10766,
#10767,#10768,#10769,#10770,#10771,#10772,#10773,#10774,#10775,#10776,#10777,
#10778,#10779,#10780,#10781,#10782,#10783,#10784,#10785,#10786,#10787,#10788,
#10789,#10790,#10791,#10792,#10793,#10794,#10795,#10796,#10797,#10798,#10799,
#10800,#10801,#10802,#10803,#10804,#10805,#10806),.UNSPECIFIED.,.F.,.F.,
(4,2,2,2,2,2,2,2,2,2,2,2,2,2,2,2,2,2,2,2,2,2,2,2,2,2,2,2,2,2,2,2,2,2,2,
2,2,2,2,2,2,2,2,2,2,2,2,2,2,2,2,2,2,2,2,2,2,2,2,2,2,2,2,2,2,2,2,2,2,2,2,
4),(1.14091205305926,1.14098686325601,1.17506124787357,1.18225125030916,
1.1865219920022,1.19083569419543,1.19822744595321,1.22321132728064,1.26980756717636,
1.28008286646988,1.28720518188926,1.29471630830586,1.3067839074636,1.34126970256588,
1.37489612603386,1.38210092847233,1.38637731973488,1.39069033933279,1.39807859739005,
1.42303310353215,1.4696683584786,1.47993497352466,1.48705464895511,1.49456566669604,
1.50663882495049,1.55441262806513,1.57671672803689,1.58293925919969,1.5869907888506,
1.5915763000801,1.60034992138208,1.6412109396252,1.67071307969318,1.68048126427172,
1.68759530647032,1.69528728204652,1.7083442745729,1.73218070338743,1.77488913957184,
1.7819634457011,1.78621221562835,1.79055226759289,1.79807644166995,1.8242397694806,
1.86877672233358,1.87932730827248,1.88649268517233,1.89392955546362,1.90560296526389,
1.91990111702837,1.95675405061808,1.97666366136682,1.9827628448936,1.98683495498047,
1.99149048806365,2.00063899654464,2.01353302438057,2.06503962186941,2.07735690524454,
2.08491173590531,2.09208562825065,2.10225501861761,2.13942737719031,2.17443185793313,
2.18157681844205,2.18583946049176,2.1901625562319,2.19760569236046,2.22305268192794,
2.26771687382351,2.27548794694238,2.28095113544787),.UNSPECIFIED.);
#143=B_SPLINE_CURVE_WITH_KNOTS('',3,(#10810,#10811,#10812,#10813,#10814,
#10815,#10816,#10817,#10818,#10819,#10820,#10821,#10822,#10823,#10824,#10825,
#10826,#10827,#10828,#10829,#10830,#10831,#10832,#10833,#10834,#10835,#10836,
#10837,#10838,#10839,#10840,#10841,#10842,#10843,#10844,#10845,#10846,#10847,
#10848,#10849,#10850,#10851,#10852,#10853,#10854,#10855,#10856,#10857,#10858,
#10859,#10860,#10861,#10862,#10863,#10864,#10865,#10866,#10867,#10868,#10869,
#10870,#10871,#10872,#10873),.UNSPECIFIED.,.F.,.F.,(4,3,3,3,3,3,3,3,3,3,
3,3,3,3,3,3,3,3,3,3,3,4),(-4.09157007060721,-3.99819923940857,-3.89835156497246,
-3.79864772858848,-3.69864794120947,-3.5991264524945,-3.4996392348841,-3.40015603967125,
-3.29977938714255,-3.20015661005484,-3.09940301980564,-2.99864942955643,
-2.89996225994261,-2.80141569488778,-2.70297985623509,-2.60460299513241,
-2.50625345286672,-2.40789960785008,-2.30944973523756,-2.2109455342352,
-2.11228415465847,-2.06679336762492),.UNSPECIFIED.);
#144=B_SPLINE_CURVE_WITH_KNOTS('',3,(#10877,#10878,#10879,#10880,#10881),
 .UNSPECIFIED.,.F.,.F.,(4,1,4),(0.,0.999549809852145,1.11662023360648),
 .UNSPECIFIED.);
#145=B_SPLINE_CURVE_WITH_KNOTS('',3,(#10883,#10884,#10885,#10886,#10887,
#10888,#10889,#10890,#10891,#10892,#10893,#10894,#10895,#10896,#10897,#10898,
#10899,#10900,#10901,#10902,#10903,#10904,#10905,#10906,#10907,#10908,#10909,
#10910,#10911,#10912,#10913,#10914,#10915,#10916,#10917,#10918,#10919,#10920,
#10921,#10922,#10923,#10924,#10925,#10926,#10927,#10928,#10929,#10930,#10931,
#10932,#10933,#10934,#10935,#10936,#10937,#10938,#10939,#10940,#10941,#10942,
#10943,#10944,#10945,#10946,#10947,#10948,#10949,#10950,#10951,#10952,#10953,
#10954,#10955,#10956,#10957,#10958,#10959,#10960,#10961,#10962,#10963,#10964,
#10965,#10966,#10967,#10968,#10969,#10970,#10971,#10972,#10973,#10974,#10975,
#10976,#10977,#10978,#10979,#10980,#10981,#10982,#10983,#10984,#10985,#10986,
#10987,#10988,#10989,#10990,#10991,#10992,#10993,#10994,#10995,#10996,#10997,
#10998,#10999,#11000,#11001,#11002,#11003,#11004,#11005,#11006,#11007,#11008,
#11009,#11010,#11011,#11012,#11013,#11014,#11015,#11016,#11017,#11018,#11019,
#11020,#11021,#11022,#11023,#11024,#11025,#11026,#11027,#11028,#11029,#11030,
#11031,#11032,#11033,#11034,#11035,#11036,#11037,#11038,#11039,#11040,#11041,
#11042,#11043,#11044,#11045,#11046,#11047,#11048,#11049,#11050,#11051,#11052,
#11053,#11054,#11055,#11056,#11057,#11058,#11059,#11060,#11061,#11062,#11063,
#11064,#11065,#11066,#11067,#11068,#11069,#11070,#11071,#11072),
 .UNSPECIFIED.,.F.,.F.,(4,3,3,3,3,3,3,3,3,3,3,3,3,3,3,3,3,3,3,3,3,3,3,3,
3,3,3,3,3,3,3,3,3,3,3,3,3,3,3,3,3,3,3,3,3,3,3,3,3,3,3,3,3,3,3,3,3,3,3,3,
3,3,3,4),(1.11662023360648,1.21415700903785,1.31227483537115,1.40958631975065,
1.50685024378918,1.60409914654667,1.70284926483607,1.8002232178696,1.89966141878694,
1.99909961970429,2.0988159569863,2.19838757899243,2.29842031031293,2.39780836260854,
2.49716197145402,2.59651155591453,2.697046024325,2.79653649081236,2.8975929601844,
2.99864942955643,3.09848076178733,3.19817176264502,3.29817519724046,3.39769245810353,
3.49717869068034,3.59666414129913,3.69704791582649,3.79668086896899,3.89744005418878,
3.99819923940857,4.09777814999803,4.19721232014855,4.29727941128758,4.39653099436606,
4.49574881322469,4.59496347522391,4.69565986873311,4.79501895395638,4.89638400160855,
4.99774904926072,5.09743314979569,5.19697375033416,5.2970143889315,5.39637464816663,
5.49570174804806,5.59502615055517,5.69559432769459,5.79506317005562,5.89618101458424,
5.99729885911286,6.09698793002092,6.19653388796859,6.29657323559314,6.3959397624514,
6.49527345959839,6.59460478137224,6.69516575327043,6.79464224294108,6.89574545595304,
6.99684866896501,7.1073445025526,7.21750034428983,7.32707552235099,7.39980554057894),
 .UNSPECIFIED.);
#146=B_SPLINE_CURVE_WITH_KNOTS('',3,(#11074,#11075,#11076,#11077,#11078,
#11079,#11080,#11081,#11082,#11083,#11084,#11085,#11086,#11087,#11088,#11089,
#11090,#11091,#11092,#11093,#11094,#11095,#11096,#11097,#11098,#11099,#11100,
#11101,#11102,#11103,#11104,#11105,#11106,#11107,#11108,#11109,#11110,#11111,
#11112,#11113,#11114,#11115,#11116,#11117,#11118,#11119,#11120,#11121,#11122,
#11123,#11124,#11125,#11126,#11127,#11128,#11129,#11130,#11131,#11132,#11133,
#11134,#11135,#11136,#11137,#11138,#11139,#11140,#11141,#11142,#11143,#11144,
#11145,#11146,#11147,#11148,#11149,#11150,#11151,#11152,#11153,#11154,#11155,
#11156,#11157,#11158,#11159,#11160,#11161,#11162,#11163,#11164,#11165,#11166,
#11167,#11168,#11169,#11170,#11171,#11172,#11173,#11174,#11175,#11176,#11177,
#11178,#11179,#11180,#11181,#11182,#11183,#11184,#11185,#11186,#11187,#11188,
#11189,#11190,#11191,#11192,#11193,#11194,#11195,#11196,#11197,#11198,#11199,
#11200,#11201,#11202,#11203,#11204,#11205,#11206,#11207,#11208,#11209,#11210,
#11211,#11212,#11213,#11214,#11215,#11216,#11217,#11218,#11219,#11220,#11221,
#11222,#11223,#11224,#11225,#11226,#11227,#11228,#11229,#11230,#11231,#11232,
#11233,#11234,#11235,#11236,#11237,#11238,#11239,#11240,#11241,#11242,#11243,
#11244,#11245,#11246,#11247,#11248,#11249,#11250,#11251,#11252,#11253,#11254,
#11255,#11256,#11257,#11258,#11259,#11260,#11261,#11262,#11263),
 .UNSPECIFIED.,.F.,.F.,(4,3,3,3,3,3,3,3,3,3,3,3,3,3,3,3,3,3,3,3,3,3,3,3,
3,3,3,3,3,3,3,3,3,3,3,3,3,3,3,3,3,3,3,3,3,3,3,3,3,3,3,3,3,3,3,3,3,3,3,3,
3,3,3,4),(7.39980554078607,7.50053108874774,7.60129313193771,7.7022021005082,
7.80318522932661,7.90438016308932,7.99639847881715,8.09607318258208,8.19560444098551,
8.29564742194599,8.39499854501913,8.49431660729804,8.59363208364627,8.69421113490202,
8.79367142016632,8.8948098544178,8.99594828866929,9.09562248122942,9.19515325722896,
9.29519636239052,9.39454707756092,9.49386476100677,9.59317988824142,9.69375944081142,
9.79321945438592,9.89435877645368,9.99549809852144,10.0951692453042,10.1946969174379,
10.2947407913049,10.3940882835689,10.4934027064381,10.5927145397381,10.693297881897,
10.7927545527067,10.8939012305401,10.9950479083736,11.0947207974823,11.1942502358541,
11.2942936711506,11.3936429749175,11.492959222287,11.5922728906363,11.6928540975337,
11.792312610642,11.8934551644338,11.9945977182257,12.0942704170841,12.1937996665268,
12.2938431492207,12.393192268754,12.4925083340807,12.5918218228387,12.6924032491485,
12.7918615906077,12.8930045593428,12.9941475280779,13.0933718526145,13.192459812771,
13.2914426505252,13.3903625391045,13.4892414456069,13.5881552424106,13.6829908479657),
 .UNSPECIFIED.);
#147=B_SPLINE_CURVE_WITH_KNOTS('',3,(#11265,#11266,#11267,#11268,#11269,
#11270,#11271,#11272,#11273,#11274,#11275,#11276,#11277,#11278,#11279,#11280,
#11281,#11282,#11283,#11284,#11285,#11286,#11287,#11288,#11289,#11290,#11291,
#11292,#11293,#11294,#11295,#11296,#11297,#11298,#11299,#11300,#11301,#11302,
#11303,#11304,#11305,#11306,#11307,#11308,#11309,#11310,#11311,#11312,#11313,
#11314,#11315,#11316,#11317,#11318,#11319,#11320,#11321,#11322,#11323,#11324,
#11325,#11326,#11327,#11328,#11329,#11330,#11331,#11332,#11333,#11334,#11335,
#11336,#11337,#11338,#11339,#11340,#11341,#11342,#11343,#11344,#11345,#11346,
#11347,#11348,#11349,#11350,#11351,#11352,#11353,#11354,#11355,#11356,#11357,
#11358,#11359,#11360,#11361,#11362,#11363,#11364,#11365,#11366,#11367,#11368,
#11369,#11370,#11371,#11372,#11373,#11374,#11375,#11376,#11377,#11378,#11379,
#11380,#11381,#11382,#11383,#11384,#11385,#11386,#11387,#11388,#11389,#11390,
#11391,#11392,#11393,#11394,#11395,#11396,#11397,#11398,#11399,#11400,#11401,
#11402,#11403,#11404,#11405,#11406,#11407,#11408,#11409,#11410,#11411,#11412,
#11413,#11414,#11415,#11416,#11417,#11418,#11419,#11420,#11421,#11422,#11423,
#11424,#11425,#11426,#11427,#11428,#11429,#11430,#11431,#11432,#11433,#11434,
#11435,#11436,#11437,#11438,#11439,#11440,#11441,#11442,#11443,#11444,#11445,
#11446,#11447,#11448,#11449,#11450,#11451,#11452,#11453,#11454),
 .UNSPECIFIED.,.F.,.F.,(4,3,3,3,3,3,3,3,3,3,3,3,3,3,3,3,3,3,3,3,3,3,3,3,
3,3,3,3,3,3,3,3,3,3,3,3,3,3,3,3,3,3,3,3,3,3,3,3,3,3,3,3,3,3,3,3,3,3,3,3,
3,3,3,4),(13.6829908483355,13.8012987037146,13.9211119521594,13.99369733793,
14.093369932917,14.1928990751328,14.292942584214,14.392291589093,14.4916075372192,
14.5909209063797,14.6915024667303,14.7909606838751,14.8921039158287,14.9932471477822,
15.0929197052539,15.1924488098593,15.2924923283312,15.3918412956528,15.4911572063268,
15.5904705381924,15.6910521430529,15.7905103236783,15.8916536406563,15.9927969576343,
16.0924694828721,16.1919985545393,16.2920420811577,16.3913910140619,16.4907068898376,
16.5900201863698,16.690601831649,16.7900599762254,16.8912033718559,16.9923467674864,
17.0920193189202,17.1915484171806,17.2915919372004,17.3909408974713,17.4902568008438,
17.5895701251662,17.6901517382093,17.7896099107689,17.8907532440537,17.9918965773386,
18.0915691226361,18.1910982147193,18.2911417362782,18.3904906903181,18.4898065874535,
18.5891199055412,18.6897015259535,18.7891596923486,18.8903030397697,18.9914463871907,
19.0907047944209,19.1898201075523,19.2888206743773,19.3877588790043,19.4866657728217,
19.5855723677555,19.6845767311066,19.7836300076881,19.8828580081811,19.9661761547613),
 .UNSPECIFIED.);
#148=B_SPLINE_CURVE_WITH_KNOTS('',3,(#11456,#11457,#11458,#11459,#11460,
#11461,#11462,#11463,#11464,#11465,#11466,#11467,#11468,#11469,#11470,#11471,
#11472,#11473,#11474,#11475,#11476,#11477,#11478,#11479,#11480,#11481,#11482,
#11483,#11484,#11485,#11486,#11487,#11488,#11489,#11490,#11491,#11492,#11493,
#11494,#11495,#11496,#11497,#11498,#11499,#11500,#11501,#11502,#11503,#11504,
#11505,#11506,#11507,#11508,#11509,#11510,#11511,#11512,#11513,#11514,#11515,
#11516,#11517,#11518,#11519,#11520,#11521,#11522,#11523,#11524,#11525,#11526,
#11527,#11528,#11529,#11530,#11531,#11532,#11533,#11534,#11535,#11536,#11537,
#11538,#11539,#11540,#11541,#11542,#11543,#11544,#11545,#11546,#11547,#11548,
#11549,#11550,#11551,#11552,#11553,#11554,#11555,#11556,#11557,#11558,#11559,
#11560,#11561,#11562,#11563,#11564,#11565,#11566,#11567,#11568,#11569,#11570,
#11571,#11572,#11573,#11574,#11575,#11576,#11577,#11578,#11579,#11580,#11581,
#11582,#11583,#11584,#11585,#11586,#11587,#11588,#11589,#11590,#11591,#11592,
#11593,#11594,#11595,#11596,#11597,#11598,#11599,#11600,#11601,#11602,#11603,
#11604,#11605,#11606,#11607,#11608,#11609,#11610,#11611,#11612,#11613,#11614,
#11615,#11616,#11617,#11618,#11619,#11620,#11621,#11622,#11623,#11624,#11625,
#11626,#11627,#11628,#11629,#11630,#11631,#11632,#11633,#11634,#11635,#11636,
#11637,#11638,#11639,#11640,#11641,#11642,#11643,#11644,#11645),
 .UNSPECIFIED.,.F.,.F.,(4,3,3,3,3,3,3,3,3,3,3,3,3,3,3,3,3,3,3,3,3,3,3,3,
3,3,3,3,3,3,3,3,3,3,3,3,3,3,3,3,3,3,3,3,3,3,3,3,3,3,3,3,3,3,3,3,3,3,3,3,
3,3,3,4),(19.9661761551452,19.9909961970429,20.0906687423831,20.1901978344841,
20.2902413560355,20.3895903100322,20.4889062071013,20.5882195250995,20.6888011455484,
20.7882593117979,20.8894026593464,20.990546006895,21.0902185513232,21.1897476425038,
21.2897911642842,21.3891401173469,21.4884560134792,21.5877693305389,21.688350952091,
21.7878091174074,21.8889524670773,21.9900958167472,22.0897683609266,22.189297451851,
22.2893409736946,22.3886899264848,22.4880058223391,22.5873191391156,22.6879007609866,
22.7873589260099,22.8885022763046,22.9896456265993,23.0893181710964,23.1888472623445,
23.2888907841079,23.3882397372341,23.4875556334283,23.5868689505481,23.6874505720239,
23.7869087373954,23.8880520869235,23.9891954364515,24.0888679808449,24.1883970719877,
24.2884405937772,24.3877895467945,24.4871054428787,24.5864187598876,24.6870003814916,
24.7864585467512,24.8876018965274,24.9887452463036,25.0884177908087,25.1879468820631,
25.2879904038247,25.387339356953,25.4866552531475,25.5859685702662,25.6865501917386,
25.7860083571051,25.8871517066304,25.9882950561557,26.1188282590924,26.2493614620292),
 .UNSPECIFIED.);
#149=B_SPLINE_CURVE_WITH_KNOTS('',3,(#11647,#11648,#11649,#11650,#11651,
#11652,#11653,#11654,#11655,#11656,#11657,#11658,#11659,#11660,#11661,#11662,
#11663,#11664,#11665,#11666,#11667,#11668,#11669,#11670,#11671,#11672,#11673,
#11674,#11675,#11676,#11677,#11678,#11679,#11680,#11681,#11682,#11683,#11684,
#11685,#11686,#11687,#11688,#11689,#11690,#11691,#11692,#11693,#11694,#11695,
#11696,#11697,#11698,#11699,#11700,#11701,#11702,#11703,#11704,#11705,#11706,
#11707,#11708,#11709,#11710,#11711,#11712,#11713,#11714,#11715,#11716,#11717,
#11718,#11719,#11720,#11721,#11722,#11723,#11724,#11725,#11726,#11727,#11728,
#11729,#11730,#11731,#11732,#11733,#11734,#11735,#11736,#11737,#11738,#11739,
#11740,#11741,#11742,#11743,#11744,#11745,#11746,#11747,#11748,#11749,#11750,
#11751,#11752,#11753,#11754,#11755,#11756,#11757,#11758,#11759,#11760,#11761,
#11762,#11763,#11764,#11765,#11766,#11767,#11768,#11769,#11770,#11771,#11772,
#11773,#11774,#11775,#11776,#11777,#11778,#11779,#11780,#11781,#11782,#11783,
#11784,#11785,#11786,#11787,#11788,#11789,#11790,#11791,#11792,#11793,#11794,
#11795,#11796,#11797,#11798,#11799,#11800,#11801,#11802,#11803,#11804,#11805,
#11806,#11807,#11808,#11809,#11810,#11811,#11812,#11813,#11814,#11815,#11816,
#11817,#11818,#11819,#11820,#11821,#11822,#11823,#11824,#11825,#11826,#11827,
#11828,#11829,#11830,#11831,#11832,#11833,#11834,#11835,#11836,#11837,#11838,
#11839),.UNSPECIFIED.,.F.,.F.,(4,3,3,3,3,3,3,3,3,3,3,3,3,3,3,3,3,3,3,3,
3,3,3,3,3,3,3,3,3,3,3,3,3,3,3,3,3,3,3,3,3,3,3,3,3,3,3,3,3,3,3,3,3,3,3,3,
3,3,3,3,3,3,3,3,4),(26.2493614623248,26.3477156658028,26.4460142361312,
26.5442888935363,26.6425713247428,26.7409564245699,26.8393988921363,26.9380064119851,
26.9878448660079,27.0875174104623,27.1870465016636,27.2870900234381,27.3864389765076,
27.4857548726413,27.5850681896973,27.685649811238,27.7851079765379,27.8862513261989,
27.98739467586,28.0870672212339,28.1865963133616,28.2866398349054,28.3859887889108,
28.4853046859821,28.5846180039758,28.6851996244099,28.7846577906385,28.8858011381754,
28.9869444857122,29.0866170277615,29.1861461165615,29.2861896389368,29.3855385896319,
29.4848544834064,29.5841677981215,29.6847494224822,29.7842075855098,29.885350940537,
29.9864942955643,30.0861668411268,30.1856959334179,30.2857394549178,30.3850884090259,
30.4844043061771,30.583717624228,30.6842992445252,30.7837574107548,30.8849007580856,
30.9860441054165,31.085716657025,31.1852457554226,31.2852892754034,31.3846382357193,
31.4839541391023,31.5832674634001,31.6838490763672,31.7833072488177,31.8844505820432,
31.9855939152686,32.0884337774174,32.1910932256562,32.2935519798997,32.3958915779211,
32.4981122183601,32.5325467695044),.UNSPECIFIED.);
#150=B_SPLINE_CURVE_WITH_KNOTS('',3,(#11841,#11842,#11843,#11844,#11845,
#11846,#11847,#11848,#11849,#11850,#11851,#11852,#11853,#11854,#11855,#11856,
#11857,#11858,#11859,#11860,#11861,#11862,#11863,#11864,#11865,#11866,#11867,
#11868,#11869,#11870,#11871,#11872,#11873,#11874,#11875,#11876,#11877,#11878,
#11879,#11880,#11881,#11882,#11883,#11884,#11885,#11886,#11887,#11888,#11889,
#11890,#11891,#11892,#11893,#11894,#11895,#11896,#11897,#11898,#11899,#11900,
#11901,#11902,#11903,#11904,#11905,#11906,#11907,#11908,#11909,#11910,#11911,
#11912,#11913,#11914,#11915,#11916,#11917,#11918,#11919,#11920,#11921,#11922,
#11923,#11924,#11925,#11926,#11927,#11928,#11929,#11930,#11931,#11932,#11933,
#11934,#11935,#11936,#11937,#11938,#11939,#11940,#11941,#11942,#11943,#11944,
#11945,#11946,#11947,#11948,#11949,#11950,#11951,#11952,#11953,#11954,#11955,
#11956,#11957,#11958,#11959,#11960,#11961,#11962,#11963,#11964,#11965,#11966,
#11967,#11968,#11969,#11970,#11971,#11972,#11973,#11974,#11975,#11976,#11977,
#11978,#11979,#11980,#11981,#11982,#11983,#11984,#11985,#11986,#11987,#11988,
#11989,#11990,#11991,#11992,#11993,#11994,#11995,#11996,#11997,#11998,#11999,
#12000,#12001,#12002,#12003,#12004,#12005,#12006,#12007,#12008,#12009,#12010,
#12011,#12012,#12013,#12014,#12015,#12016,#12017,#12018,#12019,#12020,#12021,
#12022,#12023,#12024,#12025,#12026,#12027,#12028,#12029,#12030,#12031,#12032,
#12033),.UNSPECIFIED.,.F.,.F.,(4,3,3,3,3,3,3,3,3,3,3,3,3,3,3,3,3,3,3,3,
3,3,3,3,3,3,3,3,3,3,3,3,3,3,3,3,3,3,3,3,3,3,3,3,3,3,3,3,3,3,3,3,3,3,3,3,
3,3,3,3,3,3,3,3,4),(32.5325467697432,32.6388708786208,32.7456097074644,
32.8525716002337,32.9598580208814,32.9851437251207,33.0848162851276,33.1843453917237,
33.2843889096299,33.383737877605,33.4830537884294,33.5823671199426,33.6829487237002,
33.7824069027416,33.8835502188572,33.9846935349729,34.0843661305128,34.1838952731631,
34.2839387821208,34.3832877871423,34.4826037353011,34.5819171043847,34.6824986644947,
34.7819568812939,34.8831001130595,34.984243344825,35.0839157121467,35.1834446260861,
35.28348819216,35.3828369689343,35.4821526895209,35.5814658320094,35.6820476626763,
35.781505657582,35.8826494061296,35.9837931546772,36.0834658770091,36.1829951448861,
36.2830386223415,36.382387747926,36.4817038146451,36.5810173001397,36.6815987162371,
36.7810570430293,36.8822000037793,36.9833429645293,37.0830158504659,37.1825452863463,
37.2825887223507,37.3819380253,37.4812542724812,37.5805679412715,37.681149149549,
37.7806076646393,37.8817502195104,37.9828927743815,38.0810757587581,38.1790933410021,
38.277018137445,38.3748823697557,38.4727181782476,38.5706033625315,38.6685154729089,
38.7665475575039,38.8157320763496),.UNSPECIFIED.);
#151=B_SPLINE_CURVE_WITH_KNOTS('',3,(#12035,#12036,#12037,#12038,#12039,
#12040,#12041,#12042,#12043,#12044,#12045,#12046,#12047,#12048,#12049,#12050,
#12051,#12052,#12053,#12054,#12055,#12056,#12057,#12058,#12059,#12060,#12061,
#12062,#12063,#12064,#12065,#12066,#12067,#12068,#12069,#12070,#12071,#12072,
#12073,#12074,#12075,#12076,#12077,#12078,#12079,#12080,#12081,#12082,#12083,
#12084,#12085,#12086,#12087,#12088,#12089,#12090,#12091,#12092,#12093,#12094,
#12095,#12096,#12097,#12098,#12099,#12100,#12101,#12102,#12103,#12104,#12105,
#12106,#12107,#12108,#12109,#12110,#12111,#12112,#12113,#12114,#12115,#12116,
#12117,#12118,#12119,#12120,#12121,#12122,#12123,#12124,#12125,#12126,#12127,
#12128,#12129,#12130,#12131,#12132,#12133,#12134,#12135,#12136,#12137,#12138,
#12139,#12140,#12141,#12142,#12143,#12144,#12145,#12146,#12147,#12148,#12149,
#12150,#12151,#12152,#12153,#12154,#12155,#12156,#12157,#12158,#12159,#12160,
#12161,#12162,#12163,#12164,#12165,#12166,#12167,#12168,#12169,#12170,#12171,
#12172,#12173,#12174,#12175,#12176,#12177,#12178,#12179,#12180,#12181,#12182,
#12183,#12184,#12185,#12186,#12187,#12188,#12189,#12190,#12191,#12192,#12193,
#12194,#12195,#12196,#12197,#12198,#12199,#12200,#12201,#12202,#12203,#12204,
#12205,#12206,#12207,#12208,#12209,#12210,#12211,#12212,#12213,#12214,#12215,
#12216,#12217,#12218,#12219,#12220,#12221,#12222,#12223,#12224),
 .UNSPECIFIED.,.F.,.F.,(4,3,3,3,3,3,3,3,3,3,3,3,3,3,3,3,3,3,3,3,3,3,3,3,
3,3,3,3,3,3,3,3,3,3,3,3,3,3,3,3,3,3,3,3,3,3,3,3,3,3,3,3,3,3,3,3,3,3,3,3,
3,3,3,4),(38.815732076684,38.9740421812337,38.9824425842336,39.0821169883579,
39.1816479305039,39.2816909884516,39.3810417581606,39.4803594541538,39.5796745519763,
39.6802540125036,39.779713893883,39.8808531439844,39.9819923940857,40.0816670057345,
40.1811981917972,40.2812411933147,40.3805922926417,40.4799103494576,40.5792258386122,
40.6798049299436,40.7792652727665,40.8804037383522,40.9815422039379,41.0812025067406,
41.1807193316412,41.2807659169098,41.3801026326589,41.479406329145,41.5787075003759,
41.6793036287294,41.7787499036571,41.8799209587235,41.98109201379,42.0807829495895,
42.1803303720206,42.2803693034733,42.3797363109771,42.4790701185659,42.5784011808555,
42.6789613415522,42.7784366657676,42.8795392447049,42.9806418236422,43.0803246126712,
43.1798641832779,43.279905114555,43.379265035741,43.4785920579057,43.5779166428325,
43.678485390498,43.7779550524245,43.8790733429594,43.9801916334943,44.0797657624161,
44.1791961764749,44.2792643348338,44.3785146836635,44.4777322163513,44.5769475395425,
44.6776460154935,44.7770080855589,44.8783747644527,44.9797414433465,45.0989173838636),
 .UNSPECIFIED.);
#152=B_SPLINE_CURVE_WITH_KNOTS('',3,(#12226,#12227,#12228,#12229,#12230,
#12231,#12232,#12233,#12234,#12235,#12236,#12237,#12238,#12239,#12240,#12241,
#12242,#12243,#12244,#12245,#12246,#12247,#12248,#12249,#12250,#12251,#12252,
#12253,#12254,#12255,#12256,#12257,#12258,#12259,#12260,#12261,#12262,#12263,
#12264,#12265,#12266,#12267,#12268,#12269,#12270,#12271,#12272,#12273,#12274,
#12275,#12276,#12277,#12278,#12279,#12280,#12281,#12282,#12283),
 .UNSPECIFIED.,.F.,.F.,(4,3,3,3,3,3,3,3,3,3,3,3,3,3,3,3,3,3,3,4),(45.0989173840903,
45.1972992220322,45.295544194221,45.39371339496,45.4918387659123,45.5899521922755,
45.6881513826732,45.7863907224215,45.8848024611066,45.9792912531986,46.0779782270971,
46.1765245999247,46.274960260773,46.3733369495747,46.4716863252168,46.5700400094697,
46.6684897839427,46.7669938897809,46.8656553144966,46.9113379312297),
 .UNSPECIFIED.);
#153=B_SPLINE_CURVE_WITH_KNOTS('',3,(#12287,#12288,#12289,#12290),
 .UNSPECIFIED.,.F.,.F.,(4,4),(-48.977940682755,-48.0738672208643),
 .UNSPECIFIED.);
#154=B_SPLINE_CURVE_WITH_KNOTS('',3,(#12292,#12293,#12294,#12295,#12296,
#12297,#12298,#12299,#12300,#12301,#12302),.UNSPECIFIED.,.F.,.F.,(4,1,1,
1,1,1,1,1,4),(-48.0738672208643,-47.9783908729029,-46.9788410630507,-45.9792912531986,
-44.9797414433464,-43.9801916334943,-42.9806418236422,-41.98109201379,-41.7906819136848),
 .UNSPECIFIED.);
#155=B_SPLINE_CURVE_WITH_KNOTS('',3,(#12304,#12305,#12306,#12307,#12308,
#12309,#12310,#12311,#12312,#12313,#12314,#12315,#12316,#12317,#12318,#12319,
#12320,#12321,#12322,#12323,#12324,#12325,#12326,#12327,#12328,#12329,#12330,
#12331,#12332,#12333,#12334,#12335,#12336,#12337,#12338,#12339,#12340,#12341,
#12342,#12343,#12344,#12345,#12346,#12347,#12348,#12349,#12350,#12351,#12352,
#12353,#12354,#12355,#12356,#12357,#12358,#12359,#12360,#12361,#12362,#12363,
#12364,#12365,#12366,#12367,#12368,#12369,#12370,#12371,#12372,#12373,#12374,
#12375,#12376,#12377,#12378,#12379,#12380,#12381,#12382,#12383,#12384,#12385,
#12386,#12387,#12388,#12389,#12390,#12391,#12392,#12393,#12394,#12395,#12396,
#12397,#12398,#12399,#12400,#12401,#12402,#12403,#12404,#12405,#12406,#12407,
#12408,#12409,#12410,#12411,#12412,#12413,#12414,#12415,#12416,#12417,#12418,
#12419,#12420,#12421,#12422,#12423,#12424,#12425,#12426,#12427,#12428,#12429,
#12430,#12431,#12432,#12433,#12434,#12435,#12436,#12437,#12438,#12439,#12440,
#12441,#12442,#12443,#12444,#12445,#12446,#12447,#12448,#12449,#12450,#12451,
#12452,#12453,#12454,#12455,#12456,#12457,#12458,#12459,#12460,#12461,#12462,
#12463,#12464,#12465,#12466,#12467,#12468,#12469,#12470,#12471,#12472,#12473,
#12474,#12475,#12476,#12477,#12478,#12479,#12480,#12481,#12482,#12483,#12484,
#12485,#12486,#12487,#12488,#12489,#12490,#12491,#12492,#12493,#12494,#12495,
#12496),.UNSPECIFIED.,.F.,.F.,(4,3,3,3,3,3,3,3,3,3,3,3,3,3,3,3,3,3,3,3,
3,3,3,3,3,3,3,3,3,3,3,3,3,3,3,3,3,3,3,3,3,3,3,3,3,3,3,3,3,3,3,3,3,3,3,3,
3,3,3,3,3,3,3,3,4),(-41.7906819136848,-41.6895394499664,-41.5916133636765,
-41.4937386771787,-41.3958832780933,-41.2980150835204,-41.2000434104553,
-41.1020090687524,-41.0038203197812,-40.9815422039379,-40.8818674958635,
-40.7823362331089,-40.682293253231,-40.5829421257369,-40.4836240590206,
-40.3843085782246,-40.2837295321899,-40.1842692424979,-40.0831308182918,
-39.9819923940857,-39.8823182004062,-39.7827874232564,-39.6827443183786,
-39.5833936019912,-39.484075917306,-39.3847607888111,-39.2841812376667,
-39.1847212227925,-39.083581903513,-38.9824425842336,-38.8827714393196,
-38.7832437690838,-38.683199894746,-38.5838524044374,-38.4845379835411,
-38.3852261522286,-38.2846428077668,-38.1851861389609,-38.0840394566712,
-37.9828927743814,-37.8832198845563,-37.7836904454607,-37.6836470103443,
-37.5842977058408,-37.4849814577319,-37.3856677886411,-37.2850865826131,
-37.1856280687656,-37.0844855166474,-36.9833429645293,-36.8836702655405,
-36.7841410159631,-36.6840975333024,-36.5847484136251,-36.4854323481509,
-36.3861188592427,-36.2855374331013,-36.1860790914856,-36.0849361230814,
-35.9837931546772,-35.8778143170505,-35.7721698676901,-35.666730815553,
-35.5615688752373,-35.5074966067537),.UNSPECIFIED.);
#156=B_SPLINE_CURVE_WITH_KNOTS('',3,(#12498,#12499,#12500,#12501,#12502,
#12503,#12504,#12505,#12506,#12507,#12508,#12509,#12510,#12511,#12512,#12513,
#12514,#12515,#12516,#12517,#12518,#12519,#12520,#12521,#12522,#12523,#12524,
#12525,#12526,#12527,#12528,#12529,#12530,#12531,#12532,#12533,#12534,#12535,
#12536,#12537,#12538,#12539,#12540,#12541,#12542,#12543,#12544,#12545,#12546,
#12547,#12548,#12549,#12550,#12551,#12552,#12553,#12554,#12555,#12556,#12557,
#12558,#12559,#12560,#12561,#12562,#12563,#12564,#12565,#12566,#12567,#12568,
#12569,#12570,#12571,#12572,#12573,#12574,#12575,#12576,#12577,#12578,#12579,
#12580,#12581,#12582,#12583,#12584,#12585,#12586,#12587,#12588,#12589,#12590,
#12591,#12592,#12593,#12594,#12595,#12596,#12597,#12598,#12599,#12600,#12601,
#12602,#12603,#12604,#12605,#12606,#12607,#12608,#12609,#12610,#12611,#12612,
#12613,#12614,#12615,#12616,#12617,#12618,#12619,#12620,#12621,#12622,#12623,
#12624,#12625,#12626,#12627,#12628,#12629,#12630,#12631,#12632,#12633,#12634,
#12635,#12636,#12637,#12638,#12639,#12640,#12641,#12642,#12643,#12644,#12645,
#12646,#12647,#12648,#12649,#12650,#12651,#12652,#12653,#12654,#12655,#12656,
#12657,#12658,#12659,#12660,#12661,#12662,#12663,#12664,#12665,#12666,#12667,
#12668,#12669,#12670,#12671,#12672,#12673,#12674,#12675,#12676,#12677,#12678,
#12679,#12680,#12681,#12682,#12683,#12684,#12685,#12686,#12687),
 .UNSPECIFIED.,.F.,.F.,(4,3,3,3,3,3,3,3,3,3,3,3,3,3,3,3,3,3,3,3,3,3,3,3,
3,3,3,3,3,3,3,3,3,3,3,3,3,3,3,3,3,3,3,3,3,3,3,3,3,3,3,3,3,3,3,3,3,3,3,3,
3,3,3,4),(-35.5074966065052,-35.4044188003066,-35.2993749364362,-35.195940502646,
-35.0900919237355,-34.984243344825,-34.8845707497232,-34.785041607391,-34.6849980983388,
-34.5856490933414,-34.4863331450963,-34.3870197758162,-34.2864382156054,
-34.1869799983413,-34.0858367666571,-33.9846935349729,-33.88502097749,-33.7854918728732,
-33.6854483544041,-33.5860993870697,-33.4867834763825,-33.3874701445034,
-33.2868885396577,-33.1874303590178,-33.0862870420692,-32.9851437251207,
-32.8854711999204,-32.7859421282914,-32.6858986016635,-32.5865496687987,
-32.4872337930628,-32.3879204965709,-32.2873388512453,-32.1878807067094,
-32.086737310989,-31.9855939152686,-31.8859213638172,-31.7863922655387,
-31.6863487455234,-31.5869997852342,-31.4876838818432,-31.3883705575024,
-31.2877889444809,-31.1883307719029,-31.0871874386596,-30.9860441054164,
-30.8863715601185,-30.786842468035,-30.6867989464762,-30.5874499924358,
-30.4881340952999,-30.3888207772115,-30.2882391567997,-30.1887809904039,
-30.0876376429841,-29.9864942955643,-29.8881025663735,-29.7898393529225,
-29.6916725189187,-29.5935700512061,-29.4954678707829,-29.3973701963672,
-29.2991861658934,-29.2243112993256),.UNSPECIFIED.);
#157=B_SPLINE_CURVE_WITH_KNOTS('',3,(#12689,#12690,#12691,#12692,#12693,
#12694,#12695,#12696,#12697,#12698,#12699,#12700,#12701,#12702,#12703,#12704,
#12705,#12706,#12707,#12708,#12709,#12710,#12711,#12712,#12713,#12714,#12715,
#12716,#12717,#12718,#12719,#12720,#12721,#12722,#12723,#12724,#12725,#12726,
#12727,#12728,#12729,#12730,#12731,#12732,#12733,#12734,#12735,#12736,#12737,
#12738,#12739,#12740,#12741,#12742,#12743,#12744,#12745,#12746,#12747,#12748,
#12749,#12750,#12751,#12752,#12753,#12754,#12755,#12756,#12757,#12758,#12759,
#12760,#12761,#12762,#12763,#12764,#12765,#12766,#12767,#12768,#12769,#12770,
#12771,#12772,#12773,#12774,#12775,#12776,#12777,#12778,#12779,#12780,#12781,
#12782,#12783,#12784,#12785,#12786,#12787,#12788,#12789,#12790,#12791,#12792,
#12793,#12794,#12795,#12796,#12797,#12798,#12799,#12800,#12801,#12802,#12803,
#12804,#12805,#12806,#12807,#12808,#12809,#12810,#12811,#12812,#12813,#12814,
#12815,#12816,#12817,#12818,#12819,#12820,#12821,#12822,#12823,#12824,#12825,
#12826,#12827,#12828,#12829,#12830,#12831,#12832,#12833,#12834,#12835,#12836,
#12837,#12838,#12839,#12840,#12841,#12842,#12843,#12844,#12845,#12846,#12847,
#12848,#12849,#12850,#12851,#12852,#12853,#12854,#12855,#12856,#12857,#12858,
#12859,#12860,#12861,#12862,#12863,#12864,#12865,#12866,#12867,#12868,#12869,
#12870,#12871,#12872,#12873,#12874,#12875,#12876,#12877,#12878),
 .UNSPECIFIED.,.F.,.F.,(4,3,3,3,3,3,3,3,3,3,3,3,3,3,3,3,3,3,3,3,3,3,3,3,
3,3,3,3,3,3,3,3,3,3,3,3,3,3,3,3,3,3,3,3,3,3,3,3,3,3,3,3,3,3,3,3,3,3,3,3,
3,3,3,4),(-29.2243112989953,-29.0922651704096,-28.9869444857122,-28.8872719403693,
-28.7877428482655,-28.6876993267148,-28.5883503727153,-28.4890344756434,
-28.3897211576422,-28.2891395371967,-28.1896813709443,-28.0885380234021,
-27.98739467586,-27.887722131432,-27.7881930402516,-27.6881495184711,-27.5888005654086,
-27.4894846692765,-27.3901713522169,-27.2895897306646,-27.1901315653484,
-27.0889882156781,-26.9878448660079,-26.888172321829,-26.7886432309051,
-26.6885997090615,-26.5892507562718,-26.4899348604181,-26.3906215436422,
-26.2900399217706,-26.1905817567479,-26.0894384064518,-25.9882950561557,
-25.8886225116583,-25.7890934204099,-25.6890498986466,-25.5897009455201,
-25.4903850493256,-25.3910717322055,-25.29049011073,-25.1910319453582,-25.0898885958309,
-24.9887452463036,-24.8890727019102,-24.7895436107676,-24.6895000889781,
-24.5901511359609,-24.4908352398768,-24.391521922868,-24.2909403012638,
-24.1914821360043,-24.0903387862279,-23.9891954364514,-23.889522891946,
-23.7899938006913,-23.6899502789298,-23.5906013258012,-23.4912854296062,
-23.3919721124873,-23.2913904910153,-23.1919323256484,-23.0907889761239,
-22.9896456265993,-22.941125992146),.UNSPECIFIED.);
#158=B_SPLINE_CURVE_WITH_KNOTS('',3,(#12880,#12881,#12882,#12883,#12884,
#12885,#12886,#12887,#12888,#12889,#12890,#12891,#12892,#12893,#12894,#12895,
#12896,#12897,#12898,#12899,#12900,#12901,#12902,#12903,#12904,#12905,#12906,
#12907,#12908,#12909,#12910,#12911,#12912,#12913,#12914,#12915,#12916,#12917,
#12918,#12919,#12920,#12921,#12922,#12923,#12924,#12925,#12926,#12927,#12928,
#12929,#12930,#12931,#12932,#12933,#12934,#12935,#12936,#12937,#12938,#12939,
#12940,#12941,#12942,#12943,#12944,#12945,#12946,#12947,#12948,#12949,#12950,
#12951,#12952,#12953,#12954,#12955,#12956,#12957,#12958,#12959,#12960,#12961,
#12962,#12963,#12964,#12965,#12966,#12967,#12968,#12969,#12970,#12971,#12972,
#12973,#12974,#12975,#12976,#12977,#12978,#12979,#12980,#12981,#12982,#12983,
#12984,#12985,#12986,#12987,#12988,#12989,#12990,#12991,#12992,#12993,#12994,
#12995,#12996,#12997,#12998,#12999,#13000,#13001,#13002,#13003,#13004,#13005,
#13006,#13007,#13008,#13009,#13010,#13011,#13012,#13013,#13014,#13015,#13016,
#13017,#13018,#13019,#13020,#13021,#13022,#13023,#13024,#13025,#13026,#13027,
#13028,#13029,#13030,#13031,#13032,#13033,#13034,#13035,#13036,#13037,#13038,
#13039,#13040,#13041,#13042,#13043,#13044,#13045,#13046,#13047,#13048,#13049,
#13050,#13051,#13052,#13053,#13054,#13055,#13056,#13057,#13058,#13059,#13060,
#13061,#13062,#13063,#13064,#13065,#13066,#13067,#13068,#13069),
 .UNSPECIFIED.,.F.,.F.,(4,3,3,3,3,3,3,3,3,3,3,3,3,3,3,3,3,3,3,3,3,3,3,3,
3,3,3,3,3,3,3,3,3,3,3,3,3,3,3,3,3,3,3,3,3,3,3,3,3,3,3,3,3,3,3,3,3,3,3,3,
3,3,3,4),(-22.9411259918217,-22.8422132186966,-22.7434395746755,-22.6447744362852,
-22.5461673015594,-22.4475867495727,-22.3490013949527,-22.2503151664381,
-22.1515747710859,-22.052665774763,-21.9900958167472,-21.8904232722928,
-21.7908941810916,-21.690850659317,-21.5915017062476,-21.4921858101138,
-21.3928724930579,-21.2922908715172,-21.1928327062173,-21.0916893565562,
-20.990546006895,-20.8908734615185,-20.7913443693884,-20.6913008478452,
-20.5919518938372,-20.4926359967633,-20.3933226787671,-20.292741058336,
-20.1932828921048,-20.0921395445738,-19.9909961970429,-19.891323654999,
-19.7917945662044,-19.6917510438277,-19.5924020931379,-19.4930861993685,
-19.3937728846584,-19.2931912602915,-19.193733097269,-19.0925897422298,
-18.9914463871907,-18.8917738416275,-18.7922447493354,-18.6922012278358,
-18.592852273727,-18.4935363765752,-18.3942230585238,-18.2936414382275,
-18.1941832719976,-18.0930399246681,-17.9918965773386,-17.8922240257118,
-17.7926949272958,-17.6926514073196,-17.5933024469851,-17.4939865435839,
-17.3946732192674,-17.2940916063222,-17.1946334338536,-17.09349010067,-16.9923467674864,
-16.8753468893682,-16.7595002690756,-16.6579406851814),.UNSPECIFIED.);
#159=B_SPLINE_CURVE_WITH_KNOTS('',3,(#13071,#13072,#13073,#13074,#13075,
#13076,#13077,#13078,#13079,#13080,#13081,#13082,#13083,#13084,#13085,#13086,
#13087,#13088,#13089,#13090,#13091,#13092,#13093,#13094,#13095,#13096,#13097,
#13098,#13099,#13100,#13101,#13102,#13103,#13104,#13105,#13106,#13107,#13108,
#13109,#13110,#13111,#13112,#13113,#13114,#13115,#13116,#13117,#13118,#13119,
#13120,#13121,#13122,#13123,#13124,#13125,#13126,#13127,#13128,#13129,#13130,
#13131,#13132,#13133,#13134,#13135,#13136,#13137,#13138,#13139,#13140,#13141,
#13142,#13143,#13144,#13145,#13146,#13147,#13148,#13149,#13150,#13151,#13152,
#13153,#13154,#13155,#13156,#13157,#13158,#13159,#13160,#13161,#13162,#13163,
#13164,#13165,#13166,#13167,#13168,#13169,#13170,#13171,#13172,#13173,#13174,
#13175,#13176,#13177,#13178,#13179,#13180,#13181,#13182,#13183,#13184,#13185,
#13186,#13187,#13188,#13189,#13190,#13191,#13192,#13193,#13194,#13195,#13196,
#13197,#13198,#13199,#13200,#13201,#13202,#13203,#13204,#13205,#13206,#13207,
#13208,#13209,#13210,#13211,#13212,#13213,#13214,#13215,#13216,#13217,#13218,
#13219,#13220,#13221,#13222,#13223,#13224,#13225,#13226,#13227,#13228,#13229,
#13230,#13231,#13232,#13233,#13234,#13235,#13236,#13237,#13238,#13239,#13240,
#13241,#13242,#13243,#13244,#13245,#13246,#13247,#13248,#13249,#13250,#13251,
#13252,#13253,#13254,#13255,#13256,#13257,#13258,#13259,#13260,#13261,#13262,
#13263),.UNSPECIFIED.,.F.,.F.,(4,3,3,3,3,3,3,3,3,3,3,3,3,3,3,3,3,3,3,3,
3,3,3,3,3,3,3,3,3,3,3,3,3,3,3,3,3,3,3,3,3,3,3,3,3,3,3,3,3,3,3,3,3,3,3,3,
3,3,3,3,3,3,3,3,4),(-16.6579406849664,-16.5586673411425,-16.4594098080319,
-16.3601376655488,-16.2607507488239,-16.1613029056952,-16.061674030148,
-15.9927969576343,-15.8931243976124,-15.7935952910013,-15.6935517730989,
-15.5942028051098,-15.4948868942719,-15.3955735627455,-15.2949919590046,
-15.1955337799511,-15.0943904638666,-14.9932471477821,-14.8935745521242,
-14.7940454093551,-14.694001900427,-14.5946528952861,-14.495336947008,-14.3960235778053,
-14.2954420178365,-14.1959838009197,-14.0948405694249,-13.99369733793,-13.894024970901,
-13.7944960572543,-13.6944524911072,-13.595103714624,-13.495787994327,-13.3964748521264,
-13.2958930211143,-13.1964350264896,-13.0952912772837,-12.9941475280779,
-12.8944748055864,-12.7949455375518,-12.694902060136,-12.5955529343998,
-12.4962368675317,-12.3969233818907,-12.2963419659745,-12.1968836390442,
-12.0957406786349,-11.9945977182257,-11.8949248315594,-11.7953953949446,
-11.6953519591232,-11.596002655434,-11.4966864075124,-11.3973727379825,
-11.2967915305803,-11.1973330147593,-11.0961904615665,-10.9950479083736,
-10.8944502270782,-10.7940032781318,-10.6891913030456,-10.5889704326472,
-10.4888063042122,-10.3886646483777,-10.3747553777868),.UNSPECIFIED.);
#160=B_SPLINE_CURVE_WITH_KNOTS('',3,(#13264,#13265,#13266,#13267,#13268,
#13269,#13270,#13271,#13272,#13273,#13274,#13275,#13276,#13277,#13278,#13279,
#13280,#13281,#13282,#13283,#13284,#13285,#13286,#13287,#13288,#13289,#13290,
#13291,#13292,#13293,#13294,#13295,#13296,#13297,#13298,#13299,#13300,#13301,
#13302,#13303,#13304,#13305,#13306,#13307,#13308,#13309,#13310,#13311,#13312,
#13313,#13314,#13315,#13316,#13317,#13318,#13319,#13320,#13321,#13322,#13323,
#13324,#13325,#13326,#13327,#13328,#13329,#13330,#13331,#13332,#13333,#13334,
#13335,#13336,#13337,#13338,#13339,#13340,#13341,#13342,#13343,#13344,#13345,
#13346,#13347,#13348,#13349,#13350,#13351,#13352,#13353,#13354,#13355,#13356,
#13357,#13358,#13359,#13360,#13361,#13362,#13363,#13364,#13365,#13366,#13367,
#13368,#13369,#13370,#13371,#13372,#13373,#13374,#13375,#13376,#13377,#13378,
#13379,#13380,#13381,#13382,#13383,#13384,#13385,#13386,#13387,#13388,#13389,
#13390,#13391,#13392,#13393,#13394,#13395,#13396,#13397,#13398,#13399,#13400,
#13401,#13402,#13403,#13404,#13405,#13406,#13407,#13408,#13409,#13410,#13411,
#13412,#13413,#13414,#13415,#13416,#13417,#13418,#13419,#13420,#13421,#13422,
#13423,#13424,#13425,#13426,#13427,#13428,#13429,#13430,#13431,#13432,#13433,
#13434,#13435,#13436,#13437,#13438,#13439,#13440,#13441,#13442,#13443,#13444,
#13445,#13446,#13447,#13448,#13449,#13450,#13451,#13452,#13453,#13454,#13455,
#13456),.UNSPECIFIED.,.F.,.F.,(4,3,3,3,3,3,3,3,3,3,3,3,3,3,3,3,3,3,3,3,
3,3,3,3,3,3,3,3,3,3,3,3,3,3,3,3,3,3,3,3,3,3,3,3,3,3,3,3,3,3,3,3,3,3,3,3,
3,3,3,3,3,3,3,3,4),(-10.3747553775598,-10.2633020300802,-10.1513665111728,
-10.0388261271735,-9.99549809852144,-9.8958236930791,-9.79629274962715,
-9.69624969200742,-9.59689892103024,-9.49758122378561,-9.39826612473022,
-9.29768666571498,-9.19822678315976,-9.09708753591453,-8.99594828866929,
-8.89627367265352,-8.79674248219455,-8.69669948177237,-8.5973483780097,
-8.49803031675303,-8.39871482315869,-8.29813573707331,-8.19867538985861,
-8.09753693433788,-7.99639847881715,-7.89673818865013,-7.79722137640207,
-7.69717478797244,-7.59783808482659,-7.49853440089793,-7.39923324216268,
-7.29863709886326,-7.19919083615364,-7.09801975255933,-6.99684866896501,
-6.89715772460678,-6.79761029368071,-6.69757136435973,-6.59820434857338,
-6.49887053279914,-6.3995394624311,-6.29897931160154,-6.19950397964904,
-6.09840141938095,-5.99729885911286,-5.897616043936,-5.79807644701137,-5.69803552229254,
-5.59867557456924,-5.49934852584398,-5.40002391436897,-5.29945519809191,
-5.19998550992019,-5.09886727959046,-4.99774904926072,-4.89936263245375,
-4.79838856225184,-4.70026016252175,-4.60219107760665,-4.50414935420518,
-4.4010045333635,-4.30286581258146,-4.20467026972117,-4.10633389245817,
-4.09157007083846),.UNSPECIFIED.);
#161=B_SPLINE_CURVE_WITH_KNOTS('',3,(#13459,#13460,#13461,#13462,#13463,
#13464,#13465,#13466,#13467,#13468,#13469,#13470,#13471,#13472,#13473,#13474,
#13475,#13476,#13477,#13478,#13479,#13480,#13481,#13482,#13483,#13484,#13485,
#13486,#13487,#13488,#13489,#13490,#13491,#13492,#13493,#13494,#13495,#13496,
#13497,#13498,#13499,#13500,#13501,#13502,#13503,#13504,#13505,#13506,#13507,
#13508,#13509,#13510,#13511,#13512,#13513,#13514,#13515,#13516,#13517,#13518,
#13519,#13520,#13521,#13522,#13523,#13524,#13525,#13526,#13527,#13528,#13529,
#13530,#13531,#13532,#13533,#13534,#13535,#13536,#13537,#13538,#13539,#13540,
#13541,#13542,#13543,#13544,#13545,#13546,#13547,#13548,#13549,#13550,#13551,
#13552,#13553,#13554,#13555,#13556,#13557,#13558,#13559,#13560,#13561,#13562,
#13563,#13564,#13565,#13566,#13567,#13568,#13569,#13570,#13571,#13572,#13573,
#13574,#13575,#13576,#13577,#13578,#13579,#13580,#13581,#13582,#13583,#13584,
#13585,#13586,#13587,#13588,#13589,#13590,#13591,#13592,#13593,#13594,#13595,
#13596,#13597,#13598,#13599,#13600),.UNSPECIFIED.,.F.,.F.,(4,2,2,2,2,2,
2,2,2,2,2,2,2,2,2,2,2,2,2,2,2,2,2,2,2,2,2,2,2,2,2,2,2,2,2,2,2,2,2,2,2,2,
2,2,2,2,2,2,2,2,2,2,2,2,2,2,2,2,2,2,2,2,2,2,2,2,2,2,2,2,4),(0.00344614780203521,
0.0284904809162007,0.0538827835859065,0.0686235091287068,0.0805907163808784,
0.088137184145726,0.0953647804091584,0.105948947249549,0.148809238680941,
0.174870676231912,0.182416612380744,0.186813258257199,0.191148233825763,
0.198518498889793,0.239540652573207,0.265824100780086,0.278138797633332,
0.285723990068682,0.292870302749267,0.303102561147615,0.350354141141507,
0.37701560068224,0.38337240950892,0.387492863749183,0.392033763200307,0.400628758995628,
0.442163465895457,0.46192026039917,0.476487946049621,0.484426655666293,
0.4914276555967,0.500373376773164,0.520704931735167,0.557385940501716,0.571367663036804,
0.581032891036802,0.585765491248748,0.589798436758793,0.595669021614399,
0.612777843676554,0.652219618644748,0.666914259898479,0.678822075434346,
0.686311010144705,0.693463387690597,0.70387939087316,0.749251031316509,
0.774776003909911,0.782234190550168,0.786568355294679,0.790321817980931,
0.796931037944707,0.837127218544441,0.868266394811345,0.879325378369257,
0.886654854005653,0.894008061095456,0.90519984640876,0.939888617553977,
0.975099823638863,0.982320866939109,0.986600426159565,0.99090689945427,
0.998270083153767,1.03736018233108,1.06825595227068,1.07927807583162,1.08659475677513,
1.09394298889186,1.10514182987474,1.14091205305926),.UNSPECIFIED.);
#162=B_SPLINE_CURVE_WITH_KNOTS('',3,(#13603,#13604,#13605,#13606,#13607,
#13608,#13609,#13610,#13611,#13612,#13613,#13614,#13615,#13616,#13617,#13618,
#13619,#13620,#13621,#13622,#13623,#13624,#13625,#13626,#13627,#13628,#13629,
#13630,#13631,#13632,#13633,#13634,#13635,#13636,#13637,#13638,#13639,#13640,
#13641,#13642,#13643,#13644,#13645,#13646,#13647,#13648,#13649,#13650,#13651,
#13652,#13653,#13654,#13655,#13656,#13657,#13658,#13659,#13660,#13661,#13662,
#13663,#13664,#13665,#13666,#13667,#13668,#13669,#13670,#13671,#13672,#13673,
#13674,#13675,#13676,#13677,#13678,#13679,#13680,#13681,#13682,#13683,#13684,
#13685,#13686,#13687,#13688,#13689,#13690,#13691,#13692,#13693,#13694,#13695,
#13696,#13697,#13698,#13699,#13700,#13701,#13702,#13703,#13704,#13705,#13706,
#13707,#13708,#13709,#13710,#13711,#13712,#13713,#13714,#13715,#13716,#13717,
#13718),.UNSPECIFIED.,.F.,.F.,(4,2,2,2,2,2,2,2,2,2,2,2,2,2,2,2,2,2,2,2,
2,2,2,2,2,2,2,2,2,2,2,2,2,2,2,2,2,2,2,2,2,2,2,2,2,2,2,2,2,2,2,2,2,2,2,2,
2,4),(-2.03242761728642,-2.02762265841596,-2.02074164543271,-1.99378590696461,
-1.96115676855459,-1.94888264165494,-1.94078466233113,-1.93352430127577,
-1.92153998007138,-1.87671871271659,-1.84476717116948,-1.83760222730833,
-1.83330543103495,-1.82911334753728,-1.82199209565321,-1.78922107582986,
-1.7632635939393,-1.75126440888435,-1.7410821508505,-1.73413278090626,-1.72703111694745,
-1.71602151042092,-1.67429397364971,-1.64188030443115,-1.63543654221534,
-1.63142051335166,-1.62706916372963,-1.61945826864553,-1.59000834494158,
-1.55174184931512,-1.53956017079099,-1.53197388661241,-1.5247696160083,
-1.51433383519624,-1.47029166509564,-1.444912902043,-1.43744218410541,-1.43306050649059,
-1.42871011071478,-1.42126320596611,-1.39601056521357,-1.37277625645214,
-1.35578375818058,-1.34259802423399,-1.33485159013306,-1.32769445744438,
-1.31787325536777,-1.28786256114238,-1.24733765389243,-1.23856726828699,
-1.23397102673795,-1.22992510616663,-1.22370955288778,-1.20129210256359,
-1.1753772154676,-1.15699378298739,-1.1431061302417,-1.14066834730415),
 .UNSPECIFIED.);
#163=B_SPLINE_CURVE_WITH_KNOTS('',3,(#13927,#13928,#13929,#13930,#13931,
#13932,#13933,#13934,#13935,#13936,#13937,#13938,#13939,#13940,#13941,#13942,
#13943,#13944,#13945,#13946,#13947,#13948,#13949,#13950,#13951,#13952,#13953,
#13954,#13955,#13956,#13957,#13958,#13959,#13960,#13961,#13962,#13963,#13964,
#13965,#13966,#13967,#13968,#13969,#13970,#13971,#13972,#13973,#13974,#13975,
#13976,#13977,#13978,#13979,#13980,#13981,#13982,#13983,#13984,#13985,#13986,
#13987,#13988,#13989,#13990,#13991,#13992,#13993,#13994,#13995,#13996,#13997,
#13998,#13999,#14000,#14001,#14002,#14003,#14004,#14005,#14006,#14007,#14008),
 .UNSPECIFIED.,.F.,.F.,(4,3,3,3,3,3,3,3,3,3,3,3,3,3,3,3,3,3,3,3,3,3,3,3,
3,3,3,4),(-0.461743572254199,-0.445279637544711,-0.419665409334653,-0.398766763381763,
-0.394162024454705,-0.368774962988829,-0.349177254342088,-0.339871226708548,
-0.335357168261631,-0.310607959532329,-0.286107327656323,-0.262350263015158,
-0.248443506470567,-0.244441072949281,-0.220948576203007,-0.211993293814896,
-0.187932245402815,-0.164529603299809,-0.160799747913903,-0.137491872951246,
-0.114210964158578,-0.0911177765171172,-0.0820653542879866,-0.0764306774118449,
-0.054031428691482,-0.0318872073099107,-0.0105083701393909,-7.00415783501338E-15),
 .UNSPECIFIED.);
#164=B_SPLINE_CURVE_WITH_KNOTS('',3,(#14009,#14010,#14011,#14012,#14013,
#14014,#14015,#14016,#14017,#14018,#14019,#14020,#14021,#14022,#14023,#14024,
#14025,#14026,#14027,#14028,#14029,#14030,#14031,#14032,#14033,#14034,#14035,
#14036,#14037,#14038,#14039,#14040,#14041,#14042,#14043,#14044,#14045,#14046,
#14047,#14048,#14049,#14050,#14051,#14052,#14053,#14054,#14055,#14056,#14057,
#14058,#14059,#14060,#14061,#14062,#14063,#14064,#14065,#14066,#14067,#14068,
#14069,#14070,#14071,#14072,#14073,#14074,#14075,#14076,#14077,#14078,#14079,
#14080,#14081,#14082,#14083,#14084,#14085,#14086,#14087,#14088,#14089,#14090,
#14091,#14092,#14093,#14094,#14095,#14096),.UNSPECIFIED.,.F.,.F.,(4,3,3,
3,3,3,3,3,3,3,3,3,3,3,3,3,3,3,3,3,3,3,3,3,3,3,3,3,3,4),(-0.46380305084373,
-0.450143378394066,-0.42834691099736,-0.416417514424194,-0.41061770490034,
-0.40583848098822,-0.383170125624015,-0.364752716270424,-0.357183720834536,
-0.352389301015471,-0.328937236053495,-0.305197499653431,-0.281594469780252,
-0.274956577509301,-0.271007211480475,-0.246578486425838,-0.235958639370917,
-0.212131827480764,-0.188305015590611,-0.184276201227976,-0.180478707993104,
-0.156057553901815,-0.131200496694823,-0.106091750867829,-0.0960021957213982,
-0.0910056989017407,-0.0652625445071726,-0.0394826186541935,-0.0142546737832877,
0.),.UNSPECIFIED.);
#165=B_SPLINE_CURVE_WITH_KNOTS('',3,(#14102,#14103,#14104,#14105,#14106,
#14107,#14108,#14109,#14110,#14111,#14112,#14113,#14114,#14115,#14116,#14117,
#14118,#14119,#14120,#14121,#14122,#14123,#14124,#14125,#14126,#14127,#14128,
#14129,#14130,#14131,#14132,#14133,#14134,#14135,#14136,#14137,#14138,#14139,
#14140,#14141,#14142,#14143,#14144,#14145,#14146,#14147,#14148,#14149,#14150,
#14151,#14152,#14153,#14154,#14155,#14156,#14157,#14158,#14159,#14160,#14161,
#14162,#14163,#14164,#14165,#14166,#14167,#14168,#14169,#14170,#14171,#14172,
#14173,#14174,#14175,#14176,#14177,#14178,#14179,#14180,#14181,#14182,#14183,
#14184,#14185,#14186),.UNSPECIFIED.,.F.,.F.,(4,3,3,3,3,3,3,3,3,3,3,3,3,
3,3,3,3,3,3,3,3,3,3,3,3,3,3,3,4),(-0.45699211118371,-0.445279637544697,
-0.419665409508243,-0.406685902277409,-0.398766768567209,-0.39416203748691,
-0.368775578482156,-0.349177265885345,-0.339871244646184,-0.335357179438787,
-0.31060797213875,-0.286107345244344,-0.262350291376267,-0.248443540782049,
-0.244441077482334,-0.220948588962521,-0.211993293814895,-0.187932247195927,
-0.164529607973285,-0.160799753252352,-0.137463400398657,-0.114082069442804,
-0.0911406010852215,-0.0820653229868862,-0.076430692769169,-0.0539748622314556,
-0.0318871978476813,-0.0105083424875331,0.),.UNSPECIFIED.);
#166=B_SPLINE_CURVE_WITH_KNOTS('',3,(#14396,#14397,#14398,#14399,#14400,
#14401,#14402,#14403,#14404,#14405,#14406,#14407,#14408,#14409,#14410,#14411,
#14412,#14413,#14414,#14415,#14416,#14417,#14418,#14419,#14420,#14421,#14422,
#14423,#14424,#14425,#14426,#14427,#14428,#14429,#14430,#14431,#14432,#14433,
#14434,#14435,#14436,#14437,#14438,#14439,#14440,#14441,#14442,#14443,#14444,
#14445,#14446,#14447,#14448,#14449,#14450,#14451,#14452,#14453,#14454,#14455,
#14456,#14457,#14458,#14459,#14460,#14461,#14462,#14463,#14464,#14465,#14466,
#14467,#14468,#14469,#14470,#14471,#14472,#14473,#14474,#14475,#14476,#14477,
#14478,#14479,#14480),.UNSPECIFIED.,.F.,.F.,(4,3,3,3,3,3,3,3,3,3,3,3,3,
3,3,3,3,3,3,3,3,3,3,3,3,3,3,3,4),(-0.46380305084373,-0.450143378394054,
-0.428264440755745,-0.410617883401312,-0.4058385271806,-0.383170177979863,
-0.364752761817912,-0.357183853622535,-0.352389339422303,-0.328937278005717,
-0.305197541696273,-0.281594511232344,-0.274956601237073,-0.27100723282273,
-0.246578506918939,-0.235958639370914,-0.21213183187221,-0.188305024373507,
-0.184276201248984,-0.180478707195112,-0.156127340170029,-0.131048754059854,
-0.105970167949679,-0.0960021891969689,-0.0910056975232237,-0.0652625456624386,
-0.0394826167527914,-0.0142546579228003,0.),.UNSPECIFIED.);
#167=B_SPLINE_CURVE_WITH_KNOTS('',3,(#14481,#14482,#14483,#14484),
 .UNSPECIFIED.,.F.,.F.,(4,4),(0.,0.0143039377755772),.UNSPECIFIED.);
#168=B_SPLINE_CURVE_WITH_KNOTS('',3,(#14485,#14486,#14487,#14488),
 .UNSPECIFIED.,.F.,.F.,(4,4),(0.,0.0481823570135641),.UNSPECIFIED.);
#169=SPHERICAL_SURFACE('',#1978,1.9854168202488);
#170=SPHERICAL_SURFACE('',#1980,1.9854168202488);
#171=TOROIDAL_SURFACE('',#1951,2.67974687627927,0.7);
#172=TOROIDAL_SURFACE('',#2037,3.01701820384648,0.700000000000003);
#173=TOROIDAL_SURFACE('',#2103,6.60753780880871,4.83650249899603);
#174=SHAPE_REPRESENTATION_RELATIONSHIP('SRR','None',#14576,#182);
#175=SHAPE_REPRESENTATION_RELATIONSHIP('SRR','None',#14577,#183);
#176=SHAPE_REPRESENTATION_RELATIONSHIP('SRR','None',#14578,#184);
#177=SHAPE_REPRESENTATION_RELATIONSHIP('SRR','None',#14579,#185);
#178=SHAPE_REPRESENTATION_RELATIONSHIP('SRR','None',#14580,#186);
#179=SHAPE_REPRESENTATION_RELATIONSHIP('SRR','None',#14581,#187);
#180=SHAPE_REPRESENTATION_RELATIONSHIP('SRR','None',#14582,#188);
#181=SHAPE_REPRESENTATION_RELATIONSHIP('SRR','None',#14583,#189);
#182=ADVANCED_BREP_SHAPE_REPRESENTATION('',(#198),#14536);
#183=ADVANCED_BREP_SHAPE_REPRESENTATION('',(#199),#14537);
#184=ADVANCED_BREP_SHAPE_REPRESENTATION('',(#200),#14538);
#185=ADVANCED_BREP_SHAPE_REPRESENTATION('',(#201),#14539);
#186=ADVANCED_BREP_SHAPE_REPRESENTATION('',(#202),#14540);
#187=ADVANCED_BREP_SHAPE_REPRESENTATION('',(#203),#14541);
#188=ADVANCED_BREP_SHAPE_REPRESENTATION('',(#204),#14542);
#189=ADVANCED_BREP_SHAPE_REPRESENTATION('',(#205),#14543);
#190=STYLED_ITEM('',(#14625),#198);
#191=STYLED_ITEM('',(#14626),#199);
#192=STYLED_ITEM('',(#14627),#200);
#193=STYLED_ITEM('',(#14627),#201);
#194=STYLED_ITEM('',(#14626),#202);
#195=STYLED_ITEM('',(#14627),#203);
#196=STYLED_ITEM('',(#14627),#204);
#197=STYLED_ITEM('',(#14627),#205);
#198=MANIFOLD_SOLID_BREP('Body1',#1826);
#199=MANIFOLD_SOLID_BREP('Body1',#1827);
#200=MANIFOLD_SOLID_BREP('Body1',#1828);
#201=MANIFOLD_SOLID_BREP('Body1',#1829);
#202=MANIFOLD_SOLID_BREP('Body1',#1830);
#203=MANIFOLD_SOLID_BREP('Body1',#1831);
#204=MANIFOLD_SOLID_BREP('Body1',#1832);
#205=MANIFOLD_SOLID_BREP('Body1',#1833);
#206=LINE('',#2607,#262);
#207=LINE('',#2609,#263);
#208=LINE('',#2618,#264);
#209=LINE('',#2625,#265);
#210=LINE('',#2632,#266);
#211=LINE('',#2639,#267);
#212=LINE('',#2650,#268);
#213=LINE('',#2657,#269);
#214=LINE('',#2664,#270);
#215=LINE('',#2670,#271);
#216=LINE('',#2678,#272);
#217=LINE('',#2685,#273);
#218=LINE('',#2701,#274);
#219=LINE('',#2706,#275);
#220=LINE('',#2712,#276);
#221=LINE('',#2720,#277);
#222=LINE('',#2727,#278);
#223=LINE('',#2733,#279);
#224=LINE('',#2967,#280);
#225=LINE('',#3176,#281);
#226=LINE('',#3544,#282);
#227=LINE('',#3929,#283);
#228=LINE('',#4294,#284);
#229=LINE('',#4661,#285);
#230=LINE('',#5036,#286);
#231=LINE('',#5403,#287);
#232=LINE('',#5772,#288);
#233=LINE('',#6149,#289);
#234=LINE('',#8569,#290);
#235=LINE('',#8572,#291);
#236=LINE('',#8577,#292);
#237=LINE('',#8584,#293);
#238=LINE('',#8595,#294);
#239=LINE('',#8600,#295);
#240=LINE('',#8609,#296);
#241=LINE('',#8617,#297);
#242=LINE('',#8624,#298);
#243=LINE('',#8627,#299);
#244=LINE('',#8634,#300);
#245=LINE('',#8642,#301);
#246=LINE('',#8649,#302);
#247=LINE('',#8656,#303);
#248=LINE('',#8663,#304);
#249=LINE('',#8667,#305);
#250=LINE('',#8669,#306);
#251=LINE('',#8674,#307);
#252=LINE('',#8783,#308);
#253=LINE('',#9129,#309);
#254=LINE('',#9478,#310);
#255=LINE('',#9802,#311);
#256=LINE('',#10146,#312);
#257=LINE('',#10474,#313);
#258=LINE('',#14499,#314);
#259=LINE('',#14502,#315);
#260=LINE('',#14510,#316);
#261=LINE('',#14516,#317);
#262=VECTOR('',#2146,10.0021025234003);
#263=VECTOR('',#2149,11.7021025234003);
#264=VECTOR('',#2160,10.0021025234003);
#265=VECTOR('',#2169,7.93438181172474);
#266=VECTOR('',#2178,2.72924949802694);
#267=VECTOR('',#2187,3.37974687627927);
#268=VECTOR('',#2202,1.37433660530134);
#269=VECTOR('',#2211,2.58871463782345);
#270=VECTOR('',#2222,1.25945989284257);
#271=VECTOR('',#2229,0.544851764215984);
#272=VECTOR('',#2240,1.08970352843197);
#273=VECTOR('',#2249,0.625182919763592);
#274=VECTOR('',#2270,8.93704988738917);
#275=VECTOR('',#2277,1.25945989284257);
#276=VECTOR('',#2284,8.2210249646156);
#277=VECTOR('',#2295,13.263882223741);
#278=VECTOR('',#2304,11.7021025234003);
#279=VECTOR('',#2311,1.366);
#280=VECTOR('',#2316,1.366);
#281=VECTOR('',#2319,1.366);
#282=VECTOR('',#2322,1.366);
#283=VECTOR('',#2325,1.366);
#284=VECTOR('',#2328,1.366);
#285=VECTOR('',#2331,1.366);
#286=VECTOR('',#2334,1.366);
#287=VECTOR('',#2337,1.366);
#288=VECTOR('',#2340,1.366);
#289=VECTOR('',#2343,1.366);
#290=VECTOR('',#2368,3.51922397520286);
#291=VECTOR('',#2371,3.34979916874976);
#292=VECTOR('',#2378,3.18037436229666);
#293=VECTOR('',#2387,3.71701820384649);
#294=VECTOR('',#2402,1.4890246697361);
#295=VECTOR('',#2409,2.72578406873475);
#296=VECTOR('',#2420,6.94221583892671);
#297=VECTOR('',#2431,9.77637943942299);
#298=VECTOR('',#2440,11.3384150169577);
#299=VECTOR('',#2443,11.1537701181833);
#300=VECTOR('',#2452,8.2465180845384);
#301=VECTOR('',#2463,6.03157539652109);
#302=VECTOR('',#2472,3.90337928524842);
#303=VECTOR('',#2481,2.91473371720024);
#304=VECTOR('',#2490,2.52802020062926);
#305=VECTOR('',#2495,2.14952775522097);
#306=VECTOR('',#2498,1.77103530981268);
#307=VECTOR('',#2503,1.99475);
#308=VECTOR('',#2508,1.99475);
#309=VECTOR('',#2511,1.99475);
#310=VECTOR('',#2514,1.99475);
#311=VECTOR('',#2517,1.99475);
#312=VECTOR('',#2520,1.99475);
#313=VECTOR('',#2523,1.99475);
#314=VECTOR('',#2554,3.86373699625103);
#315=VECTOR('',#2557,3.70051543670999);
#316=VECTOR('',#2568,0.684464879973279);
#317=VECTOR('',#2577,1.77103530981268);
#318=CYLINDRICAL_SURFACE('',#1931,10.0021025234003);
#319=CYLINDRICAL_SURFACE('',#1932,11.7021025234003);
#320=CYLINDRICAL_SURFACE('',#1936,10.0021025234003);
#321=CYLINDRICAL_SURFACE('',#1941,7.93438181172474);
#322=CYLINDRICAL_SURFACE('',#1945,2.72924949802694);
#323=CYLINDRICAL_SURFACE('',#1949,3.37974687627927);
#324=CYLINDRICAL_SURFACE('',#1956,1.37433660530134);
#325=CYLINDRICAL_SURFACE('',#1960,2.58871463782345);
#326=CYLINDRICAL_SURFACE('',#1965,1.25945989284257);
#327=CYLINDRICAL_SURFACE('',#1967,0.544851764215984);
#328=CYLINDRICAL_SURFACE('',#1972,1.08970352843197);
#329=CYLINDRICAL_SURFACE('',#1976,0.625182919763592);
#330=CYLINDRICAL_SURFACE('',#1986,8.93704988738917);
#331=CYLINDRICAL_SURFACE('',#1990,1.25945989284257);
#332=CYLINDRICAL_SURFACE('',#1992,8.2210249646156);
#333=CYLINDRICAL_SURFACE('',#1997,13.263882223741);
#334=CYLINDRICAL_SURFACE('',#2001,11.7021025234003);
#335=CYLINDRICAL_SURFACE('',#2005,1.366);
#336=CYLINDRICAL_SURFACE('',#2007,1.366);
#337=CYLINDRICAL_SURFACE('',#2008,1.366);
#338=CYLINDRICAL_SURFACE('',#2009,1.366);
#339=CYLINDRICAL_SURFACE('',#2010,1.366);
#340=CYLINDRICAL_SURFACE('',#2011,1.366);
#341=CYLINDRICAL_SURFACE('',#2012,1.366);
#342=CYLINDRICAL_SURFACE('',#2013,1.366);
#343=CYLINDRICAL_SURFACE('',#2014,1.366);
#344=CYLINDRICAL_SURFACE('',#2015,1.366);
#345=CYLINDRICAL_SURFACE('',#2016,1.366);
#346=CYLINDRICAL_SURFACE('',#2017,1.70825);
#347=CYLINDRICAL_SURFACE('',#2020,1.366);
#348=CYLINDRICAL_SURFACE('',#2027,3.51922397520286);
#349=CYLINDRICAL_SURFACE('',#2031,3.18037436229666);
#350=CYLINDRICAL_SURFACE('',#2035,3.71701820384649);
#351=CYLINDRICAL_SURFACE('',#2042,1.4890246697361);
#352=CYLINDRICAL_SURFACE('',#2046,2.72578406873475);
#353=CYLINDRICAL_SURFACE('',#2059,11.3384150169577);
#354=CYLINDRICAL_SURFACE('',#2069,6.03157539652109);
#355=CYLINDRICAL_SURFACE('',#2077,2.91473371720024);
#356=CYLINDRICAL_SURFACE('',#2081,2.52802020062926);
#357=CYLINDRICAL_SURFACE('',#2085,1.77103530981268);
#358=CYLINDRICAL_SURFACE('',#2087,1.99475);
#359=CYLINDRICAL_SURFACE('',#2089,1.99475);
#360=CYLINDRICAL_SURFACE('',#2090,1.99475);
#361=CYLINDRICAL_SURFACE('',#2091,1.99475);
#362=CYLINDRICAL_SURFACE('',#2092,1.99475);
#363=CYLINDRICAL_SURFACE('',#2093,1.99475);
#364=CYLINDRICAL_SURFACE('',#2094,1.99475);
#365=CYLINDRICAL_SURFACE('',#2095,2.4505);
#366=CYLINDRICAL_SURFACE('',#2098,1.99475);
#367=CYLINDRICAL_SURFACE('',#2108,3.86373699625103);
#368=CYLINDRICAL_SURFACE('',#2114,0.684464879973279);
#369=CYLINDRICAL_SURFACE('',#2119,1.77103530981268);
#370=FACE_BOUND('',#505,.T.);
#371=FACE_BOUND('',#507,.T.);
#372=FACE_BOUND('',#513,.T.);
#373=FACE_BOUND('',#516,.T.);
#374=FACE_BOUND('',#519,.T.);
#375=FACE_BOUND('',#523,.T.);
#376=FACE_BOUND('',#526,.T.);
#377=FACE_BOUND('',#530,.T.);
#378=FACE_BOUND('',#534,.T.);
#379=FACE_BOUND('',#537,.T.);
#380=FACE_BOUND('',#542,.T.);
#381=FACE_BOUND('',#545,.T.);
#382=FACE_BOUND('',#549,.T.);
#383=FACE_BOUND('',#552,.T.);
#384=FACE_BOUND('',#555,.T.);
#385=FACE_BOUND('',#574,.T.);
#386=FACE_BOUND('',#579,.T.);
#387=FACE_BOUND('',#583,.T.);
#388=FACE_BOUND('',#586,.T.);
#389=FACE_BOUND('',#589,.T.);
#390=FACE_BOUND('',#592,.T.);
#391=FACE_BOUND('',#595,.T.);
#392=FACE_BOUND('',#599,.T.);
#393=FACE_BOUND('',#602,.T.);
#394=FACE_BOUND('',#605,.T.);
#395=FACE_BOUND('',#608,.T.);
#396=FACE_BOUND('',#611,.T.);
#397=FACE_BOUND('',#629,.T.);
#398=FACE_BOUND('',#633,.T.);
#399=FACE_OUTER_BOUND('',#504,.T.);
#400=FACE_OUTER_BOUND('',#506,.T.);
#401=FACE_OUTER_BOUND('',#508,.T.);
#402=FACE_OUTER_BOUND('',#509,.T.);
#403=FACE_OUTER_BOUND('',#510,.T.);
#404=FACE_OUTER_BOUND('',#511,.T.);
#405=FACE_OUTER_BOUND('',#512,.T.);
#406=FACE_OUTER_BOUND('',#514,.T.);
#407=FACE_OUTER_BOUND('',#515,.T.);
#408=FACE_OUTER_BOUND('',#517,.T.);
#409=FACE_OUTER_BOUND('',#518,.T.);
#410=FACE_OUTER_BOUND('',#520,.T.);
#411=FACE_OUTER_BOUND('',#521,.T.);
#412=FACE_OUTER_BOUND('',#522,.T.);
#413=FACE_OUTER_BOUND('',#524,.T.);
#414=FACE_OUTER_BOUND('',#525,.T.);
#415=FACE_OUTER_BOUND('',#527,.T.);
#416=FACE_OUTER_BOUND('',#528,.T.);
#417=FACE_OUTER_BOUND('',#529,.T.);
#418=FACE_OUTER_BOUND('',#531,.T.);
#419=FACE_OUTER_BOUND('',#532,.T.);
#420=FACE_OUTER_BOUND('',#533,.T.);
#421=FACE_OUTER_BOUND('',#535,.T.);
#422=FACE_OUTER_BOUND('',#536,.T.);
#423=FACE_OUTER_BOUND('',#538,.T.);
#424=FACE_OUTER_BOUND('',#539,.T.);
#425=FACE_OUTER_BOUND('',#540,.T.);
#426=FACE_OUTER_BOUND('',#541,.T.);
#427=FACE_OUTER_BOUND('',#543,.T.);
#428=FACE_OUTER_BOUND('',#544,.T.);
#429=FACE_OUTER_BOUND('',#546,.T.);
#430=FACE_OUTER_BOUND('',#547,.T.);
#431=FACE_OUTER_BOUND('',#548,.T.);
#432=FACE_OUTER_BOUND('',#550,.T.);
#433=FACE_OUTER_BOUND('',#551,.T.);
#434=FACE_OUTER_BOUND('',#553,.T.);
#435=FACE_OUTER_BOUND('',#554,.T.);
#436=FACE_OUTER_BOUND('',#556,.T.);
#437=FACE_OUTER_BOUND('',#557,.T.);
#438=FACE_OUTER_BOUND('',#558,.T.);
#439=FACE_OUTER_BOUND('',#559,.T.);
#440=FACE_OUTER_BOUND('',#560,.T.);
#441=FACE_OUTER_BOUND('',#561,.T.);
#442=FACE_OUTER_BOUND('',#562,.T.);
#443=FACE_OUTER_BOUND('',#563,.T.);
#444=FACE_OUTER_BOUND('',#564,.T.);
#445=FACE_OUTER_BOUND('',#565,.T.);
#446=FACE_OUTER_BOUND('',#566,.T.);
#447=FACE_OUTER_BOUND('',#567,.T.);
#448=FACE_OUTER_BOUND('',#568,.T.);
#449=FACE_OUTER_BOUND('',#569,.T.);
#450=FACE_OUTER_BOUND('',#570,.T.);
#451=FACE_OUTER_BOUND('',#571,.T.);
#452=FACE_OUTER_BOUND('',#572,.T.);
#453=FACE_OUTER_BOUND('',#573,.T.);
#454=FACE_OUTER_BOUND('',#575,.T.);
#455=FACE_OUTER_BOUND('',#576,.T.);
#456=FACE_OUTER_BOUND('',#577,.T.);
#457=FACE_OUTER_BOUND('',#578,.T.);
#458=FACE_OUTER_BOUND('',#580,.T.);
#459=FACE_OUTER_BOUND('',#581,.T.);
#460=FACE_OUTER_BOUND('',#582,.T.);
#461=FACE_OUTER_BOUND('',#584,.T.);
#462=FACE_OUTER_BOUND('',#585,.T.);
#463=FACE_OUTER_BOUND('',#587,.T.);
#464=FACE_OUTER_BOUND('',#588,.T.);
#465=FACE_OUTER_BOUND('',#590,.T.);
#466=FACE_OUTER_BOUND('',#591,.T.);
#467=FACE_OUTER_BOUND('',#593,.T.);
#468=FACE_OUTER_BOUND('',#594,.T.);
#469=FACE_OUTER_BOUND('',#596,.T.);
#470=FACE_OUTER_BOUND('',#597,.T.);
#471=FACE_OUTER_BOUND('',#598,.T.);
#472=FACE_OUTER_BOUND('',#600,.T.);
#473=FACE_OUTER_BOUND('',#601,.T.);
#474=FACE_OUTER_BOUND('',#603,.T.);
#475=FACE_OUTER_BOUND('',#604,.T.);
#476=FACE_OUTER_BOUND('',#606,.T.);
#477=FACE_OUTER_BOUND('',#607,.T.);
#478=FACE_OUTER_BOUND('',#609,.T.);
#479=FACE_OUTER_BOUND('',#610,.T.);
#480=FACE_OUTER_BOUND('',#612,.T.);
#481=FACE_OUTER_BOUND('',#613,.T.);
#482=FACE_OUTER_BOUND('',#614,.T.);
#483=FACE_OUTER_BOUND('',#615,.T.);
#484=FACE_OUTER_BOUND('',#616,.T.);
#485=FACE_OUTER_BOUND('',#617,.T.);
#486=FACE_OUTER_BOUND('',#618,.T.);
#487=FACE_OUTER_BOUND('',#619,.T.);
#488=FACE_OUTER_BOUND('',#620,.T.);
#489=FACE_OUTER_BOUND('',#621,.T.);
#490=FACE_OUTER_BOUND('',#622,.T.);
#491=FACE_OUTER_BOUND('',#623,.T.);
#492=FACE_OUTER_BOUND('',#624,.T.);
#493=FACE_OUTER_BOUND('',#625,.T.);
#494=FACE_OUTER_BOUND('',#626,.T.);
#495=FACE_OUTER_BOUND('',#627,.T.);
#496=FACE_OUTER_BOUND('',#628,.T.);
#497=FACE_OUTER_BOUND('',#630,.T.);
#498=FACE_OUTER_BOUND('',#631,.T.);
#499=FACE_OUTER_BOUND('',#632,.T.);
#500=FACE_OUTER_BOUND('',#634,.T.);
#501=FACE_OUTER_BOUND('',#635,.T.);
#502=FACE_OUTER_BOUND('',#636,.T.);
#503=FACE_OUTER_BOUND('',#637,.T.);
#504=EDGE_LOOP('',(#1171));
#505=EDGE_LOOP('',(#1172));
#506=EDGE_LOOP('',(#1173));
#507=EDGE_LOOP('',(#1174));
#508=EDGE_LOOP('',(#1175,#1176,#1177,#1178));
#509=EDGE_LOOP('',(#1179,#1180,#1181,#1182));
#510=EDGE_LOOP('',(#1183));
#511=EDGE_LOOP('',(#1184,#1185,#1186,#1187));
#512=EDGE_LOOP('',(#1188));
#513=EDGE_LOOP('',(#1189));
#514=EDGE_LOOP('',(#1190,#1191,#1192,#1193));
#515=EDGE_LOOP('',(#1194));
#516=EDGE_LOOP('',(#1195));
#517=EDGE_LOOP('',(#1196,#1197,#1198,#1199));
#518=EDGE_LOOP('',(#1200));
#519=EDGE_LOOP('',(#1201));
#520=EDGE_LOOP('',(#1202,#1203,#1204,#1205));
#521=EDGE_LOOP('',(#1206,#1207,#1208,#1209));
#522=EDGE_LOOP('',(#1210));
#523=EDGE_LOOP('',(#1211));
#524=EDGE_LOOP('',(#1212,#1213,#1214,#1215));
#525=EDGE_LOOP('',(#1216));
#526=EDGE_LOOP('',(#1217));
#527=EDGE_LOOP('',(#1218,#1219,#1220,#1221));
#528=EDGE_LOOP('',(#1222));
#529=EDGE_LOOP('',(#1223));
#530=EDGE_LOOP('',(#1224));
#531=EDGE_LOOP('',(#1225,#1226,#1227,#1228));
#532=EDGE_LOOP('',(#1229,#1230,#1231,#1232));
#533=EDGE_LOOP('',(#1233));
#534=EDGE_LOOP('',(#1234));
#535=EDGE_LOOP('',(#1235,#1236,#1237,#1238));
#536=EDGE_LOOP('',(#1239));
#537=EDGE_LOOP('',(#1240));
#538=EDGE_LOOP('',(#1241,#1242,#1243,#1244));
#539=EDGE_LOOP('',(#1245,#1246,#1247));
#540=EDGE_LOOP('',(#1248,#1249,#1250));
#541=EDGE_LOOP('',(#1251));
#542=EDGE_LOOP('',(#1252));
#543=EDGE_LOOP('',(#1253,#1254,#1255,#1256));
#544=EDGE_LOOP('',(#1257));
#545=EDGE_LOOP('',(#1258));
#546=EDGE_LOOP('',(#1259,#1260,#1261,#1262));
#547=EDGE_LOOP('',(#1263,#1264,#1265,#1266));
#548=EDGE_LOOP('',(#1267));
#549=EDGE_LOOP('',(#1268));
#550=EDGE_LOOP('',(#1269,#1270,#1271,#1272));
#551=EDGE_LOOP('',(#1273));
#552=EDGE_LOOP('',(#1274));
#553=EDGE_LOOP('',(#1275,#1276,#1277,#1278));
#554=EDGE_LOOP('',(#1279));
#555=EDGE_LOOP('',(#1280));
#556=EDGE_LOOP('',(#1281,#1282,#1283,#1284));
#557=EDGE_LOOP('',(#1285,#1286,#1287,#1288,#1289,#1290));
#558=EDGE_LOOP('',(#1291,#1292,#1293,#1294,#1295));
#559=EDGE_LOOP('',(#1296,#1297,#1298,#1299,#1300));
#560=EDGE_LOOP('',(#1301,#1302,#1303,#1304,#1305));
#561=EDGE_LOOP('',(#1306,#1307,#1308,#1309,#1310));
#562=EDGE_LOOP('',(#1311,#1312,#1313,#1314,#1315));
#563=EDGE_LOOP('',(#1316,#1317,#1318,#1319,#1320));
#564=EDGE_LOOP('',(#1321,#1322,#1323,#1324,#1325));
#565=EDGE_LOOP('',(#1326,#1327,#1328,#1329,#1330));
#566=EDGE_LOOP('',(#1331,#1332,#1333,#1334,#1335));
#567=EDGE_LOOP('',(#1336,#1337,#1338,#1339,#1340,#1341,#1342,#1343,#1344,
#1345,#1346,#1347,#1348,#1349,#1350,#1351,#1352,#1353,#1354,#1355,#1356,
#1357,#1358,#1359,#1360,#1361,#1362,#1363));
#568=EDGE_LOOP('',(#1364,#1365,#1366,#1367,#1368));
#569=EDGE_LOOP('',(#1369,#1370,#1371,#1372,#1373,#1374,#1375,#1376,#1377,
#1378,#1379,#1380,#1381,#1382,#1383,#1384,#1385,#1386,#1387,#1388,#1389,
#1390,#1391,#1392,#1393,#1394,#1395,#1396,#1397,#1398,#1399,#1400,#1401));
#570=EDGE_LOOP('',(#1402,#1403,#1404,#1405,#1406,#1407,#1408,#1409,#1410,
#1411,#1412,#1413,#1414,#1415,#1416,#1417,#1418,#1419,#1420,#1421,#1422,
#1423,#1424,#1425,#1426,#1427,#1428,#1429,#1430,#1431,#1432,#1433,#1434,
#1435));
#571=EDGE_LOOP('',(#1436));
#572=EDGE_LOOP('',(#1437,#1438,#1439,#1440));
#573=EDGE_LOOP('',(#1441));
#574=EDGE_LOOP('',(#1442,#1443,#1444,#1445,#1446));
#575=EDGE_LOOP('',(#1447,#1448,#1449,#1450));
#576=EDGE_LOOP('',(#1451,#1452,#1453,#1454));
#577=EDGE_LOOP('',(#1455,#1456,#1457,#1458));
#578=EDGE_LOOP('',(#1459));
#579=EDGE_LOOP('',(#1460));
#580=EDGE_LOOP('',(#1461,#1462,#1463,#1464));
#581=EDGE_LOOP('',(#1465,#1466,#1467,#1468));
#582=EDGE_LOOP('',(#1469));
#583=EDGE_LOOP('',(#1470));
#584=EDGE_LOOP('',(#1471,#1472,#1473,#1474));
#585=EDGE_LOOP('',(#1475));
#586=EDGE_LOOP('',(#1476));
#587=EDGE_LOOP('',(#1477,#1478,#1479,#1480));
#588=EDGE_LOOP('',(#1481));
#589=EDGE_LOOP('',(#1482));
#590=EDGE_LOOP('',(#1483,#1484,#1485,#1486));
#591=EDGE_LOOP('',(#1487));
#592=EDGE_LOOP('',(#1488));
#593=EDGE_LOOP('',(#1489,#1490,#1491,#1492));
#594=EDGE_LOOP('',(#1493));
#595=EDGE_LOOP('',(#1494));
#596=EDGE_LOOP('',(#1495,#1496,#1497,#1498));
#597=EDGE_LOOP('',(#1499,#1500,#1501,#1502));
#598=EDGE_LOOP('',(#1503));
#599=EDGE_LOOP('',(#1504));
#600=EDGE_LOOP('',(#1505,#1506,#1507,#1508));
#601=EDGE_LOOP('',(#1509));
#602=EDGE_LOOP('',(#1510));
#603=EDGE_LOOP('',(#1511,#1512,#1513,#1514));
#604=EDGE_LOOP('',(#1515));
#605=EDGE_LOOP('',(#1516));
#606=EDGE_LOOP('',(#1517,#1518,#1519,#1520));
#607=EDGE_LOOP('',(#1521));
#608=EDGE_LOOP('',(#1522));
#609=EDGE_LOOP('',(#1523,#1524,#1525,#1526));
#610=EDGE_LOOP('',(#1527));
#611=EDGE_LOOP('',(#1528));
#612=EDGE_LOOP('',(#1529,#1530,#1531,#1532));
#613=EDGE_LOOP('',(#1533,#1534,#1535,#1536));
#614=EDGE_LOOP('',(#1537,#1538,#1539,#1540));
#615=EDGE_LOOP('',(#1541,#1542,#1543,#1544));
#616=EDGE_LOOP('',(#1545,#1546,#1547,#1548,#1549));
#617=EDGE_LOOP('',(#1550,#1551,#1552,#1553,#1554,#1555));
#618=EDGE_LOOP('',(#1556,#1557,#1558,#1559));
#619=EDGE_LOOP('',(#1560,#1561,#1562,#1563,#1564,#1565));
#620=EDGE_LOOP('',(#1566,#1567,#1568,#1569));
#621=EDGE_LOOP('',(#1570,#1571,#1572,#1573,#1574,#1575));
#622=EDGE_LOOP('',(#1576,#1577,#1578,#1579,#1580,#1581,#1582,#1583,#1584,
#1585,#1586,#1587,#1588,#1589,#1590,#1591,#1592,#1593,#1594,#1595));
#623=EDGE_LOOP('',(#1596,#1597,#1598,#1599));
#624=EDGE_LOOP('',(#1600,#1601,#1602,#1603,#1604,#1605,#1606,#1607,#1608,
#1609,#1610,#1611,#1612,#1613,#1614,#1615,#1616,#1617,#1618,#1619,#1620,
#1621,#1622));
#625=EDGE_LOOP('',(#1623,#1624,#1625,#1626,#1627));
#626=EDGE_LOOP('',(#1628,#1629,#1630,#1631,#1632,#1633,#1634,#1635,#1636,
#1637,#1638,#1639,#1640,#1641,#1642,#1643,#1644,#1645,#1646,#1647,#1648,
#1649,#1650,#1651));
#627=EDGE_LOOP('',(#1652,#1653,#1654,#1655,#1656,#1657,#1658));
#628=EDGE_LOOP('',(#1659));
#629=EDGE_LOOP('',(#1660,#1661,#1662,#1663,#1664));
#630=EDGE_LOOP('',(#1665,#1666,#1667,#1668));
#631=EDGE_LOOP('',(#1669,#1670,#1671,#1672));
#632=EDGE_LOOP('',(#1673));
#633=EDGE_LOOP('',(#1674));
#634=EDGE_LOOP('',(#1675,#1676,#1677,#1678));
#635=EDGE_LOOP('',(#1679));
#636=EDGE_LOOP('',(#1680));
#637=EDGE_LOOP('',(#1681,#1682,#1683,#1684));
#638=CIRCLE('',#1926,11.7021025234003);
#639=CIRCLE('',#1927,10.0021025234003);
#640=CIRCLE('',#1929,11.7021025234003);
#641=CIRCLE('',#1930,10.0021025234003);
#642=CIRCLE('',#1935,1.25945989284257);
#643=CIRCLE('',#1937,10.0021025234003);
#644=CIRCLE('',#1938,10.0021025234003);
#645=CIRCLE('',#1940,7.93438181172474);
#646=CIRCLE('',#1942,7.93438181172474);
#647=CIRCLE('',#1944,2.72924949802694);
#648=CIRCLE('',#1946,2.72924949802694);
#649=CIRCLE('',#1948,3.37974687627927);
#650=CIRCLE('',#1950,3.37974687627927);
#651=CIRCLE('',#1952,0.7);
#652=CIRCLE('',#1953,2.67974687627927);
#653=CIRCLE('',#1955,1.37433660530134);
#654=CIRCLE('',#1957,1.37433660530134);
#655=CIRCLE('',#1959,2.58871463782345);
#656=CIRCLE('',#1961,2.58871463782345);
#657=CIRCLE('',#1964,1.25945989284257);
#658=CIRCLE('',#1968,0.544851764215984);
#659=CIRCLE('',#1969,0.544851764215984);
#660=CIRCLE('',#1971,1.08970352843197);
#661=CIRCLE('',#1973,1.08970352843197);
#662=CIRCLE('',#1975,0.625182919763592);
#663=CIRCLE('',#1977,0.625182919763592);
#664=CIRCLE('',#1979,1.9854168202488);
#665=CIRCLE('',#1981,1.9854168202488);
#666=CIRCLE('',#1984,8.93704988738917);
#667=CIRCLE('',#1985,1.25945989284257);
#668=CIRCLE('',#1987,8.93704988738917);
#669=CIRCLE('',#1989,1.25945989284257);
#670=CIRCLE('',#1993,8.2210249646156);
#671=CIRCLE('',#1994,8.2210249646156);
#672=CIRCLE('',#1996,13.263882223741);
#673=CIRCLE('',#1998,13.263882223741);
#674=CIRCLE('',#2000,11.7021025234003);
#675=CIRCLE('',#2002,11.7021025234003);
#676=CIRCLE('',#2006,1.366);
#677=CIRCLE('',#2018,1.70825);
#678=CIRCLE('',#2019,1.70825);
#679=CIRCLE('',#2021,1.366);
#680=CIRCLE('',#2023,2.72578406873475);
#681=CIRCLE('',#2026,3.51922397520286);
#682=CIRCLE('',#2028,3.51922397520286);
#683=CIRCLE('',#2030,3.18037436229666);
#684=CIRCLE('',#2032,3.18037436229666);
#685=CIRCLE('',#2034,3.71701820384649);
#686=CIRCLE('',#2036,3.71701820384649);
#687=CIRCLE('',#2038,3.01701820384649);
#688=CIRCLE('',#2039,0.700000000000003);
#689=CIRCLE('',#2041,1.4890246697361);
#690=CIRCLE('',#2043,1.4890246697361);
#691=CIRCLE('',#2045,2.72578406873475);
#692=CIRCLE('',#2049,6.73223109314486);
#693=CIRCLE('',#2050,1.77103530981268);
#694=CIRCLE('',#2052,7.15220058470855);
#695=CIRCLE('',#2054,9.55065635544564);
#696=CIRCLE('',#2056,10.0021025234003);
#697=CIRCLE('',#2058,11.3384150169577);
#698=CIRCLE('',#2060,11.3384150169577);
#699=CIRCLE('',#2062,10.9691252194088);
#700=CIRCLE('',#2064,8.63028983493237);
#701=CIRCLE('',#2066,7.86274633414444);
#702=CIRCLE('',#2068,6.03157539652109);
#703=CIRCLE('',#2070,6.03157539652109);
#704=CIRCLE('',#2072,4.0030788546633);
#705=CIRCLE('',#2074,3.80367971583355);
#706=CIRCLE('',#2076,2.91473371720024);
#707=CIRCLE('',#2078,2.91473371720024);
#708=CIRCLE('',#2080,2.52802020062926);
#709=CIRCLE('',#2082,2.52802020062926);
#710=CIRCLE('',#2084,1.77103530981268);
#711=CIRCLE('',#2088,1.99475);
#712=CIRCLE('',#2096,2.4505);
#713=CIRCLE('',#2097,2.4505);
#714=CIRCLE('',#2099,1.99475);
#715=CIRCLE('',#2101,2.4505);
#716=CIRCLE('',#2102,2.4505);
#717=CIRCLE('',#2104,4.83650249899603);
#718=CIRCLE('',#2105,1.77103530981268);
#719=CIRCLE('',#2107,3.86373699625103);
#720=CIRCLE('',#2109,3.86373699625103);
#721=CIRCLE('',#2111,3.53729387716894);
#722=CIRCLE('',#2113,0.684464879973279);
#723=CIRCLE('',#2115,0.684464879973279);
#724=CIRCLE('',#2118,1.77103530981268);
#725=VERTEX_POINT('',#2597);
#726=VERTEX_POINT('',#2599);
#727=VERTEX_POINT('',#2602);
#728=VERTEX_POINT('',#2604);
#729=VERTEX_POINT('',#2612);
#730=VERTEX_POINT('',#2615);
#731=VERTEX_POINT('',#2617);
#732=VERTEX_POINT('',#2621);
#733=VERTEX_POINT('',#2624);
#734=VERTEX_POINT('',#2628);
#735=VERTEX_POINT('',#2631);
#736=VERTEX_POINT('',#2635);
#737=VERTEX_POINT('',#2638);
#738=VERTEX_POINT('',#2642);
#739=VERTEX_POINT('',#2646);
#740=VERTEX_POINT('',#2649);
#741=VERTEX_POINT('',#2653);
#742=VERTEX_POINT('',#2656);
#743=VERTEX_POINT('',#2661);
#744=VERTEX_POINT('',#2667);
#745=VERTEX_POINT('',#2669);
#746=VERTEX_POINT('',#2673);
#747=VERTEX_POINT('',#2676);
#748=VERTEX_POINT('',#2680);
#749=VERTEX_POINT('',#2683);
#750=VERTEX_POINT('',#2687);
#751=VERTEX_POINT('',#2690);
#752=VERTEX_POINT('',#2694);
#753=VERTEX_POINT('',#2696);
#754=VERTEX_POINT('',#2699);
#755=VERTEX_POINT('',#2703);
#756=VERTEX_POINT('',#2709);
#757=VERTEX_POINT('',#2711);
#758=VERTEX_POINT('',#2715);
#759=VERTEX_POINT('',#2718);
#760=VERTEX_POINT('',#2722);
#761=VERTEX_POINT('',#2725);
#762=VERTEX_POINT('',#2731);
#763=VERTEX_POINT('',#2732);
#764=VERTEX_POINT('',#2734);
#765=VERTEX_POINT('',#2865);
#766=VERTEX_POINT('',#2965);
#767=VERTEX_POINT('',#2966);
#768=VERTEX_POINT('',#2968);
#769=VERTEX_POINT('',#3147);
#770=VERTEX_POINT('',#3174);
#771=VERTEX_POINT('',#3175);
#772=VERTEX_POINT('',#3369);
#773=VERTEX_POINT('',#3542);
#774=VERTEX_POINT('',#3543);
#775=VERTEX_POINT('',#3545);
#776=VERTEX_POINT('',#3927);
#777=VERTEX_POINT('',#3928);
#778=VERTEX_POINT('',#4110);
#779=VERTEX_POINT('',#4292);
#780=VERTEX_POINT('',#4293);
#781=VERTEX_POINT('',#4295);
#782=VERTEX_POINT('',#4659);
#783=VERTEX_POINT('',#4660);
#784=VERTEX_POINT('',#4846);
#785=VERTEX_POINT('',#5034);
#786=VERTEX_POINT('',#5035);
#787=VERTEX_POINT('',#5037);
#788=VERTEX_POINT('',#5401);
#789=VERTEX_POINT('',#5402);
#790=VERTEX_POINT('',#5586);
#791=VERTEX_POINT('',#5770);
#792=VERTEX_POINT('',#5771);
#793=VERTEX_POINT('',#5773);
#794=VERTEX_POINT('',#6147);
#795=VERTEX_POINT('',#6148);
#796=VERTEX_POINT('',#6326);
#797=VERTEX_POINT('',#6512);
#798=VERTEX_POINT('',#6513);
#799=VERTEX_POINT('',#6520);
#800=VERTEX_POINT('',#6522);
#801=VERTEX_POINT('',#6528);
#802=VERTEX_POINT('',#6704);
#803=VERTEX_POINT('',#6880);
#804=VERTEX_POINT('',#6892);
#805=VERTEX_POINT('',#6903);
#806=VERTEX_POINT('',#6914);
#807=VERTEX_POINT('',#6926);
#808=VERTEX_POINT('',#6937);
#809=VERTEX_POINT('',#6948);
#810=VERTEX_POINT('',#6961);
#811=VERTEX_POINT('',#6972);
#812=VERTEX_POINT('',#6984);
#813=VERTEX_POINT('',#6990);
#814=VERTEX_POINT('',#6992);
#815=VERTEX_POINT('',#7021);
#816=VERTEX_POINT('',#7033);
#817=VERTEX_POINT('',#7044);
#818=VERTEX_POINT('',#7056);
#819=VERTEX_POINT('',#7067);
#820=VERTEX_POINT('',#7078);
#821=VERTEX_POINT('',#7090);
#822=VERTEX_POINT('',#7101);
#823=VERTEX_POINT('',#7112);
#824=VERTEX_POINT('',#7124);
#825=VERTEX_POINT('',#7311);
#826=VERTEX_POINT('',#7466);
#827=VERTEX_POINT('',#7468);
#828=VERTEX_POINT('',#8384);
#829=VERTEX_POINT('',#8560);
#830=VERTEX_POINT('',#8564);
#831=VERTEX_POINT('',#8567);
#832=VERTEX_POINT('',#8571);
#833=VERTEX_POINT('',#8575);
#834=VERTEX_POINT('',#8579);
#835=VERTEX_POINT('',#8582);
#836=VERTEX_POINT('',#8586);
#837=VERTEX_POINT('',#8590);
#838=VERTEX_POINT('',#8593);
#839=VERTEX_POINT('',#8597);
#840=VERTEX_POINT('',#8603);
#841=VERTEX_POINT('',#8605);
#842=VERTEX_POINT('',#8608);
#843=VERTEX_POINT('',#8612);
#844=VERTEX_POINT('',#8615);
#845=VERTEX_POINT('',#8619);
#846=VERTEX_POINT('',#8622);
#847=VERTEX_POINT('',#8626);
#848=VERTEX_POINT('',#8630);
#849=VERTEX_POINT('',#8633);
#850=VERTEX_POINT('',#8637);
#851=VERTEX_POINT('',#8640);
#852=VERTEX_POINT('',#8644);
#853=VERTEX_POINT('',#8647);
#854=VERTEX_POINT('',#8651);
#855=VERTEX_POINT('',#8654);
#856=VERTEX_POINT('',#8658);
#857=VERTEX_POINT('',#8661);
#858=VERTEX_POINT('',#8665);
#859=VERTEX_POINT('',#8672);
#860=VERTEX_POINT('',#8673);
#861=VERTEX_POINT('',#8675);
#862=VERTEX_POINT('',#8684);
#863=VERTEX_POINT('',#8781);
#864=VERTEX_POINT('',#8782);
#865=VERTEX_POINT('',#8784);
#866=VERTEX_POINT('',#9127);
#867=VERTEX_POINT('',#9128);
#868=VERTEX_POINT('',#9130);
#869=VERTEX_POINT('',#9300);
#870=VERTEX_POINT('',#9476);
#871=VERTEX_POINT('',#9477);
#872=VERTEX_POINT('',#9800);
#873=VERTEX_POINT('',#9801);
#874=VERTEX_POINT('',#9803);
#875=VERTEX_POINT('',#9968);
#876=VERTEX_POINT('',#10144);
#877=VERTEX_POINT('',#10145);
#878=VERTEX_POINT('',#10472);
#879=VERTEX_POINT('',#10473);
#880=VERTEX_POINT('',#10475);
#881=VERTEX_POINT('',#10640);
#882=VERTEX_POINT('',#10808);
#883=VERTEX_POINT('',#10809);
#884=VERTEX_POINT('',#10874);
#885=VERTEX_POINT('',#10876);
#886=VERTEX_POINT('',#10882);
#887=VERTEX_POINT('',#11073);
#888=VERTEX_POINT('',#11264);
#889=VERTEX_POINT('',#11455);
#890=VERTEX_POINT('',#11646);
#891=VERTEX_POINT('',#11840);
#892=VERTEX_POINT('',#12034);
#893=VERTEX_POINT('',#12225);
#894=VERTEX_POINT('',#12284);
#895=VERTEX_POINT('',#12286);
#896=VERTEX_POINT('',#12291);
#897=VERTEX_POINT('',#12303);
#898=VERTEX_POINT('',#12497);
#899=VERTEX_POINT('',#12688);
#900=VERTEX_POINT('',#12879);
#901=VERTEX_POINT('',#13070);
#902=VERTEX_POINT('',#13458);
#903=VERTEX_POINT('',#13601);
#904=VERTEX_POINT('',#14098);
#905=VERTEX_POINT('',#14100);
#906=VERTEX_POINT('',#14395);
#907=VERTEX_POINT('',#14490);
#908=VERTEX_POINT('',#14494);
#909=VERTEX_POINT('',#14497);
#910=VERTEX_POINT('',#14501);
#911=VERTEX_POINT('',#14505);
#912=VERTEX_POINT('',#14508);
#913=VERTEX_POINT('',#14513);
#914=EDGE_CURVE('',#725,#725,#638,.T.);
#915=EDGE_CURVE('',#726,#726,#639,.T.);
#916=EDGE_CURVE('',#727,#727,#640,.T.);
#917=EDGE_CURVE('',#728,#728,#641,.T.);
#918=EDGE_CURVE('',#728,#726,#206,.T.);
#919=EDGE_CURVE('',#725,#727,#207,.T.);
#920=EDGE_CURVE('',#729,#729,#642,.T.);
#921=EDGE_CURVE('',#730,#730,#643,.T.);
#922=EDGE_CURVE('',#730,#731,#208,.T.);
#923=EDGE_CURVE('',#731,#731,#644,.T.);
#924=EDGE_CURVE('',#732,#732,#645,.T.);
#925=EDGE_CURVE('',#732,#733,#209,.T.);
#926=EDGE_CURVE('',#733,#733,#646,.T.);
#927=EDGE_CURVE('',#734,#734,#647,.T.);
#928=EDGE_CURVE('',#734,#735,#210,.T.);
#929=EDGE_CURVE('',#735,#735,#648,.T.);
#930=EDGE_CURVE('',#736,#736,#649,.T.);
#931=EDGE_CURVE('',#736,#737,#211,.T.);
#932=EDGE_CURVE('',#737,#737,#650,.T.);
#933=EDGE_CURVE('',#737,#738,#651,.T.);
#934=EDGE_CURVE('',#738,#738,#652,.T.);
#935=EDGE_CURVE('',#739,#739,#653,.T.);
#936=EDGE_CURVE('',#739,#740,#212,.T.);
#937=EDGE_CURVE('',#740,#740,#654,.T.);
#938=EDGE_CURVE('',#741,#741,#655,.T.);
#939=EDGE_CURVE('',#741,#742,#213,.T.);
#940=EDGE_CURVE('',#742,#742,#656,.T.);
#941=EDGE_CURVE('',#743,#743,#657,.T.);
#942=EDGE_CURVE('',#729,#743,#214,.T.);
#943=EDGE_CURVE('',#744,#744,#658,.T.);
#944=EDGE_CURVE('',#744,#745,#215,.T.);
#945=EDGE_CURVE('',#745,#745,#659,.T.);
#946=EDGE_CURVE('',#746,#746,#660,.T.);
#947=EDGE_CURVE('',#747,#747,#661,.T.);
#948=EDGE_CURVE('',#747,#746,#216,.T.);
#949=EDGE_CURVE('',#748,#748,#662,.T.);
#950=EDGE_CURVE('',#749,#749,#663,.T.);
#951=EDGE_CURVE('',#749,#748,#217,.T.);
#952=EDGE_CURVE('',#750,#749,#664,.T.);
#953=EDGE_CURVE('',#745,#751,#665,.T.);
#954=EDGE_CURVE('',#752,#752,#666,.T.);
#955=EDGE_CURVE('',#753,#753,#667,.T.);
#956=EDGE_CURVE('',#754,#754,#668,.T.);
#957=EDGE_CURVE('',#754,#752,#218,.T.);
#958=EDGE_CURVE('',#755,#755,#669,.T.);
#959=EDGE_CURVE('',#753,#755,#219,.T.);
#960=EDGE_CURVE('',#756,#756,#670,.T.);
#961=EDGE_CURVE('',#756,#757,#220,.T.);
#962=EDGE_CURVE('',#757,#757,#671,.T.);
#963=EDGE_CURVE('',#758,#758,#672,.T.);
#964=EDGE_CURVE('',#759,#759,#673,.T.);
#965=EDGE_CURVE('',#759,#758,#221,.T.);
#966=EDGE_CURVE('',#760,#760,#674,.T.);
#967=EDGE_CURVE('',#761,#761,#675,.T.);
#968=EDGE_CURVE('',#761,#760,#222,.T.);
#969=EDGE_CURVE('',#762,#763,#223,.T.);
#970=EDGE_CURVE('',#764,#762,#55,.T.);
#971=EDGE_CURVE('',#765,#764,#676,.T.);
#972=EDGE_CURVE('',#765,#763,#56,.T.);
#973=EDGE_CURVE('',#766,#767,#224,.T.);
#974=EDGE_CURVE('',#768,#766,#57,.F.);
#975=EDGE_CURVE('',#762,#768,#58,.T.);
#976=EDGE_CURVE('',#763,#769,#59,.T.);
#977=EDGE_CURVE('',#769,#767,#60,.T.);
#978=EDGE_CURVE('',#770,#771,#225,.T.);
#979=EDGE_CURVE('',#766,#770,#61,.F.);
#980=EDGE_CURVE('',#767,#772,#62,.T.);
#981=EDGE_CURVE('',#772,#771,#63,.T.);
#982=EDGE_CURVE('',#773,#774,#226,.T.);
#983=EDGE_CURVE('',#775,#773,#64,.F.);
#984=EDGE_CURVE('',#770,#775,#65,.F.);
#985=EDGE_CURVE('',#771,#774,#66,.T.);
#986=EDGE_CURVE('',#776,#777,#227,.T.);
#987=EDGE_CURVE('',#773,#776,#67,.F.);
#988=EDGE_CURVE('',#774,#778,#68,.T.);
#989=EDGE_CURVE('',#778,#777,#69,.T.);
#990=EDGE_CURVE('',#779,#780,#228,.T.);
#991=EDGE_CURVE('',#781,#779,#70,.F.);
#992=EDGE_CURVE('',#776,#781,#71,.F.);
#993=EDGE_CURVE('',#777,#780,#72,.T.);
#994=EDGE_CURVE('',#782,#783,#229,.T.);
#995=EDGE_CURVE('',#779,#782,#73,.F.);
#996=EDGE_CURVE('',#780,#784,#74,.T.);
#997=EDGE_CURVE('',#784,#783,#75,.T.);
#998=EDGE_CURVE('',#785,#786,#230,.T.);
#999=EDGE_CURVE('',#787,#785,#76,.F.);
#1000=EDGE_CURVE('',#782,#787,#77,.F.);
#1001=EDGE_CURVE('',#783,#786,#78,.T.);
#1002=EDGE_CURVE('',#788,#789,#231,.T.);
#1003=EDGE_CURVE('',#785,#788,#79,.F.);
#1004=EDGE_CURVE('',#786,#790,#80,.T.);
#1005=EDGE_CURVE('',#790,#789,#81,.T.);
#1006=EDGE_CURVE('',#791,#792,#232,.T.);
#1007=EDGE_CURVE('',#793,#791,#82,.F.);
#1008=EDGE_CURVE('',#788,#793,#83,.F.);
#1009=EDGE_CURVE('',#789,#792,#84,.T.);
#1010=EDGE_CURVE('',#794,#795,#233,.T.);
#1011=EDGE_CURVE('',#791,#794,#85,.F.);
#1012=EDGE_CURVE('',#792,#796,#86,.T.);
#1013=EDGE_CURVE('',#796,#795,#87,.F.);
#1014=EDGE_CURVE('',#797,#798,#88,.T.);
#1015=EDGE_CURVE('',#798,#799,#677,.T.);
#1016=EDGE_CURVE('',#799,#800,#89,.T.);
#1017=EDGE_CURVE('',#800,#801,#90,.T.);
#1018=EDGE_CURVE('',#801,#802,#91,.T.);
#1019=EDGE_CURVE('',#802,#803,#92,.T.);
#1020=EDGE_CURVE('',#803,#804,#93,.T.);
#1021=EDGE_CURVE('',#804,#805,#94,.T.);
#1022=EDGE_CURVE('',#805,#806,#95,.T.);
#1023=EDGE_CURVE('',#806,#807,#96,.T.);
#1024=EDGE_CURVE('',#807,#808,#97,.T.);
#1025=EDGE_CURVE('',#808,#809,#98,.T.);
#1026=EDGE_CURVE('',#809,#810,#99,.T.);
#1027=EDGE_CURVE('',#810,#811,#100,.T.);
#1028=EDGE_CURVE('',#811,#812,#101,.T.);
#1029=EDGE_CURVE('',#813,#812,#678,.T.);
#1030=EDGE_CURVE('',#813,#814,#102,.T.);
#1031=EDGE_CURVE('',#814,#815,#103,.T.);
#1032=EDGE_CURVE('',#815,#816,#104,.T.);
#1033=EDGE_CURVE('',#816,#817,#105,.T.);
#1034=EDGE_CURVE('',#817,#818,#106,.T.);
#1035=EDGE_CURVE('',#818,#819,#107,.T.);
#1036=EDGE_CURVE('',#819,#820,#108,.T.);
#1037=EDGE_CURVE('',#820,#821,#109,.T.);
#1038=EDGE_CURVE('',#821,#822,#110,.T.);
#1039=EDGE_CURVE('',#822,#823,#111,.T.);
#1040=EDGE_CURVE('',#823,#824,#112,.T.);
#1041=EDGE_CURVE('',#824,#797,#113,.T.);
#1042=EDGE_CURVE('',#795,#825,#114,.F.);
#1043=EDGE_CURVE('',#826,#825,#679,.T.);
#1044=EDGE_CURVE('',#827,#826,#115,.T.);
#1045=EDGE_CURVE('',#794,#827,#116,.F.);
#1046=EDGE_CURVE('',#812,#826,#117,.T.);
#1047=EDGE_CURVE('',#764,#799,#118,.T.);
#1048=EDGE_CURVE('',#828,#813,#119,.T.);
#1049=EDGE_CURVE('',#825,#828,#120,.T.);
#1050=EDGE_CURVE('',#798,#765,#121,.T.);
#1051=EDGE_CURVE('',#829,#829,#680,.T.);
#1052=EDGE_CURVE('',#830,#830,#681,.T.);
#1053=EDGE_CURVE('',#831,#831,#682,.T.);
#1054=EDGE_CURVE('',#831,#830,#234,.T.);
#1055=EDGE_CURVE('',#831,#832,#235,.T.);
#1056=EDGE_CURVE('',#832,#832,#683,.T.);
#1057=EDGE_CURVE('',#833,#833,#684,.T.);
#1058=EDGE_CURVE('',#833,#832,#236,.T.);
#1059=EDGE_CURVE('',#834,#834,#685,.T.);
#1060=EDGE_CURVE('',#835,#835,#686,.T.);
#1061=EDGE_CURVE('',#835,#834,#237,.T.);
#1062=EDGE_CURVE('',#836,#836,#687,.T.);
#1063=EDGE_CURVE('',#836,#835,#688,.T.);
#1064=EDGE_CURVE('',#837,#837,#689,.T.);
#1065=EDGE_CURVE('',#838,#838,#690,.T.);
#1066=EDGE_CURVE('',#838,#837,#238,.T.);
#1067=EDGE_CURVE('',#839,#839,#691,.T.);
#1068=EDGE_CURVE('',#829,#839,#239,.T.);
#1069=EDGE_CURVE('',#840,#840,#692,.T.);
#1070=EDGE_CURVE('',#841,#841,#693,.T.);
#1071=EDGE_CURVE('',#840,#842,#240,.T.);
#1072=EDGE_CURVE('',#842,#842,#694,.T.);
#1073=EDGE_CURVE('',#843,#843,#695,.T.);
#1074=EDGE_CURVE('',#844,#844,#696,.T.);
#1075=EDGE_CURVE('',#844,#843,#241,.T.);
#1076=EDGE_CURVE('',#845,#845,#697,.T.);
#1077=EDGE_CURVE('',#846,#846,#698,.T.);
#1078=EDGE_CURVE('',#846,#845,#242,.T.);
#1079=EDGE_CURVE('',#846,#847,#243,.T.);
#1080=EDGE_CURVE('',#847,#847,#699,.T.);
#1081=EDGE_CURVE('',#848,#848,#700,.T.);
#1082=EDGE_CURVE('',#848,#849,#244,.T.);
#1083=EDGE_CURVE('',#849,#849,#701,.T.);
#1084=EDGE_CURVE('',#850,#850,#702,.T.);
#1085=EDGE_CURVE('',#851,#851,#703,.T.);
#1086=EDGE_CURVE('',#851,#850,#245,.T.);
#1087=EDGE_CURVE('',#852,#852,#704,.T.);
#1088=EDGE_CURVE('',#853,#853,#705,.T.);
#1089=EDGE_CURVE('',#853,#852,#246,.T.);
#1090=EDGE_CURVE('',#854,#854,#706,.T.);
#1091=EDGE_CURVE('',#855,#855,#707,.T.);
#1092=EDGE_CURVE('',#855,#854,#247,.T.);
#1093=EDGE_CURVE('',#856,#856,#708,.T.);
#1094=EDGE_CURVE('',#857,#857,#709,.T.);
#1095=EDGE_CURVE('',#857,#856,#248,.T.);
#1096=EDGE_CURVE('',#858,#858,#710,.T.);
#1097=EDGE_CURVE('',#858,#857,#249,.T.);
#1098=EDGE_CURVE('',#841,#858,#250,.T.);
#1099=EDGE_CURVE('',#859,#860,#251,.T.);
#1100=EDGE_CURVE('',#861,#859,#122,.T.);
#1101=EDGE_CURVE('',#862,#861,#711,.T.);
#1102=EDGE_CURVE('',#862,#860,#123,.T.);
#1103=EDGE_CURVE('',#863,#864,#252,.T.);
#1104=EDGE_CURVE('',#865,#863,#124,.T.);
#1105=EDGE_CURVE('',#859,#865,#125,.T.);
#1106=EDGE_CURVE('',#860,#864,#126,.T.);
#1107=EDGE_CURVE('',#866,#867,#253,.T.);
#1108=EDGE_CURVE('',#868,#866,#127,.F.);
#1109=EDGE_CURVE('',#863,#868,#128,.T.);
#1110=EDGE_CURVE('',#864,#869,#129,.T.);
#1111=EDGE_CURVE('',#869,#867,#130,.T.);
#1112=EDGE_CURVE('',#870,#871,#254,.T.);
#1113=EDGE_CURVE('',#866,#870,#131,.F.);
#1114=EDGE_CURVE('',#867,#871,#132,.T.);
#1115=EDGE_CURVE('',#872,#873,#255,.T.);
#1116=EDGE_CURVE('',#874,#872,#133,.F.);
#1117=EDGE_CURVE('',#870,#874,#134,.F.);
#1118=EDGE_CURVE('',#871,#875,#135,.T.);
#1119=EDGE_CURVE('',#875,#873,#136,.T.);
#1120=EDGE_CURVE('',#876,#877,#256,.T.);
#1121=EDGE_CURVE('',#872,#876,#137,.F.);
#1122=EDGE_CURVE('',#873,#877,#138,.T.);
#1123=EDGE_CURVE('',#878,#879,#257,.T.);
#1124=EDGE_CURVE('',#880,#878,#139,.F.);
#1125=EDGE_CURVE('',#876,#880,#140,.F.);
#1126=EDGE_CURVE('',#877,#881,#141,.T.);
#1127=EDGE_CURVE('',#881,#879,#142,.F.);
#1128=EDGE_CURVE('',#882,#883,#143,.T.);
#1129=EDGE_CURVE('',#883,#884,#712,.T.);
#1130=EDGE_CURVE('',#884,#885,#144,.T.);
#1131=EDGE_CURVE('',#885,#886,#145,.T.);
#1132=EDGE_CURVE('',#886,#887,#146,.T.);
#1133=EDGE_CURVE('',#887,#888,#147,.T.);
#1134=EDGE_CURVE('',#888,#889,#148,.T.);
#1135=EDGE_CURVE('',#889,#890,#149,.T.);
#1136=EDGE_CURVE('',#890,#891,#150,.T.);
#1137=EDGE_CURVE('',#891,#892,#151,.T.);
#1138=EDGE_CURVE('',#892,#893,#152,.T.);
#1139=EDGE_CURVE('',#894,#893,#713,.T.);
#1140=EDGE_CURVE('',#894,#895,#153,.T.);
#1141=EDGE_CURVE('',#895,#896,#154,.T.);
#1142=EDGE_CURVE('',#896,#897,#155,.T.);
#1143=EDGE_CURVE('',#897,#898,#156,.T.);
#1144=EDGE_CURVE('',#898,#899,#157,.T.);
#1145=EDGE_CURVE('',#899,#900,#158,.T.);
#1146=EDGE_CURVE('',#900,#901,#159,.T.);
#1147=EDGE_CURVE('',#901,#882,#160,.T.);
#1148=EDGE_CURVE('',#879,#902,#161,.F.);
#1149=EDGE_CURVE('',#903,#902,#714,.T.);
#1150=EDGE_CURVE('',#878,#903,#162,.F.);
#1151=EDGE_CURVE('',#893,#903,#163,.T.);
#1152=EDGE_CURVE('',#861,#884,#164,.T.);
#1153=EDGE_CURVE('',#884,#904,#715,.T.);
#1154=EDGE_CURVE('',#904,#905,#716,.T.);
#1155=EDGE_CURVE('',#905,#862,#165,.T.);
#1156=EDGE_CURVE('',#906,#894,#166,.T.);
#1157=EDGE_CURVE('',#902,#906,#167,.T.);
#1158=EDGE_CURVE('',#905,#883,#168,.T.);
#1159=EDGE_CURVE('',#904,#907,#717,.T.);
#1160=EDGE_CURVE('',#907,#907,#718,.T.);
#1161=EDGE_CURVE('',#908,#908,#719,.T.);
#1162=EDGE_CURVE('',#909,#909,#720,.T.);
#1163=EDGE_CURVE('',#909,#908,#258,.T.);
#1164=EDGE_CURVE('',#909,#910,#259,.T.);
#1165=EDGE_CURVE('',#910,#910,#721,.T.);
#1166=EDGE_CURVE('',#911,#911,#722,.T.);
#1167=EDGE_CURVE('',#912,#912,#723,.T.);
#1168=EDGE_CURVE('',#912,#911,#260,.T.);
#1169=EDGE_CURVE('',#913,#913,#724,.T.);
#1170=EDGE_CURVE('',#907,#913,#261,.T.);
#1171=ORIENTED_EDGE('',*,*,#914,.T.);
#1172=ORIENTED_EDGE('',*,*,#915,.F.);
#1173=ORIENTED_EDGE('',*,*,#916,.F.);
#1174=ORIENTED_EDGE('',*,*,#917,.T.);
#1175=ORIENTED_EDGE('',*,*,#917,.F.);
#1176=ORIENTED_EDGE('',*,*,#918,.T.);
#1177=ORIENTED_EDGE('',*,*,#915,.T.);
#1178=ORIENTED_EDGE('',*,*,#918,.F.);
#1179=ORIENTED_EDGE('',*,*,#914,.F.);
#1180=ORIENTED_EDGE('',*,*,#919,.T.);
#1181=ORIENTED_EDGE('',*,*,#916,.T.);
#1182=ORIENTED_EDGE('',*,*,#919,.F.);
#1183=ORIENTED_EDGE('',*,*,#920,.T.);
#1184=ORIENTED_EDGE('',*,*,#921,.F.);
#1185=ORIENTED_EDGE('',*,*,#922,.T.);
#1186=ORIENTED_EDGE('',*,*,#923,.T.);
#1187=ORIENTED_EDGE('',*,*,#922,.F.);
#1188=ORIENTED_EDGE('',*,*,#923,.F.);
#1189=ORIENTED_EDGE('',*,*,#924,.T.);
#1190=ORIENTED_EDGE('',*,*,#924,.F.);
#1191=ORIENTED_EDGE('',*,*,#925,.T.);
#1192=ORIENTED_EDGE('',*,*,#926,.T.);
#1193=ORIENTED_EDGE('',*,*,#925,.F.);
#1194=ORIENTED_EDGE('',*,*,#926,.F.);
#1195=ORIENTED_EDGE('',*,*,#927,.T.);
#1196=ORIENTED_EDGE('',*,*,#927,.F.);
#1197=ORIENTED_EDGE('',*,*,#928,.T.);
#1198=ORIENTED_EDGE('',*,*,#929,.T.);
#1199=ORIENTED_EDGE('',*,*,#928,.F.);
#1200=ORIENTED_EDGE('',*,*,#930,.T.);
#1201=ORIENTED_EDGE('',*,*,#929,.F.);
#1202=ORIENTED_EDGE('',*,*,#930,.F.);
#1203=ORIENTED_EDGE('',*,*,#931,.T.);
#1204=ORIENTED_EDGE('',*,*,#932,.T.);
#1205=ORIENTED_EDGE('',*,*,#931,.F.);
#1206=ORIENTED_EDGE('',*,*,#932,.F.);
#1207=ORIENTED_EDGE('',*,*,#933,.T.);
#1208=ORIENTED_EDGE('',*,*,#934,.T.);
#1209=ORIENTED_EDGE('',*,*,#933,.F.);
#1210=ORIENTED_EDGE('',*,*,#934,.F.);
#1211=ORIENTED_EDGE('',*,*,#935,.T.);
#1212=ORIENTED_EDGE('',*,*,#935,.F.);
#1213=ORIENTED_EDGE('',*,*,#936,.T.);
#1214=ORIENTED_EDGE('',*,*,#937,.T.);
#1215=ORIENTED_EDGE('',*,*,#936,.F.);
#1216=ORIENTED_EDGE('',*,*,#938,.T.);
#1217=ORIENTED_EDGE('',*,*,#937,.F.);
#1218=ORIENTED_EDGE('',*,*,#938,.F.);
#1219=ORIENTED_EDGE('',*,*,#939,.T.);
#1220=ORIENTED_EDGE('',*,*,#940,.T.);
#1221=ORIENTED_EDGE('',*,*,#939,.F.);
#1222=ORIENTED_EDGE('',*,*,#940,.F.);
#1223=ORIENTED_EDGE('',*,*,#921,.T.);
#1224=ORIENTED_EDGE('',*,*,#941,.T.);
#1225=ORIENTED_EDGE('',*,*,#920,.F.);
#1226=ORIENTED_EDGE('',*,*,#942,.T.);
#1227=ORIENTED_EDGE('',*,*,#941,.F.);
#1228=ORIENTED_EDGE('',*,*,#942,.F.);
#1229=ORIENTED_EDGE('',*,*,#943,.F.);
#1230=ORIENTED_EDGE('',*,*,#944,.T.);
#1231=ORIENTED_EDGE('',*,*,#945,.T.);
#1232=ORIENTED_EDGE('',*,*,#944,.F.);
#1233=ORIENTED_EDGE('',*,*,#946,.F.);
#1234=ORIENTED_EDGE('',*,*,#943,.T.);
#1235=ORIENTED_EDGE('',*,*,#947,.F.);
#1236=ORIENTED_EDGE('',*,*,#948,.T.);
#1237=ORIENTED_EDGE('',*,*,#946,.T.);
#1238=ORIENTED_EDGE('',*,*,#948,.F.);
#1239=ORIENTED_EDGE('',*,*,#947,.T.);
#1240=ORIENTED_EDGE('',*,*,#949,.F.);
#1241=ORIENTED_EDGE('',*,*,#950,.F.);
#1242=ORIENTED_EDGE('',*,*,#951,.T.);
#1243=ORIENTED_EDGE('',*,*,#949,.T.);
#1244=ORIENTED_EDGE('',*,*,#951,.F.);
#1245=ORIENTED_EDGE('',*,*,#950,.T.);
#1246=ORIENTED_EDGE('',*,*,#952,.F.);
#1247=ORIENTED_EDGE('',*,*,#952,.T.);
#1248=ORIENTED_EDGE('',*,*,#945,.F.);
#1249=ORIENTED_EDGE('',*,*,#953,.T.);
#1250=ORIENTED_EDGE('',*,*,#953,.F.);
#1251=ORIENTED_EDGE('',*,*,#954,.F.);
#1252=ORIENTED_EDGE('',*,*,#955,.F.);
#1253=ORIENTED_EDGE('',*,*,#956,.F.);
#1254=ORIENTED_EDGE('',*,*,#957,.T.);
#1255=ORIENTED_EDGE('',*,*,#954,.T.);
#1256=ORIENTED_EDGE('',*,*,#957,.F.);
#1257=ORIENTED_EDGE('',*,*,#956,.T.);
#1258=ORIENTED_EDGE('',*,*,#958,.F.);
#1259=ORIENTED_EDGE('',*,*,#955,.T.);
#1260=ORIENTED_EDGE('',*,*,#959,.T.);
#1261=ORIENTED_EDGE('',*,*,#958,.T.);
#1262=ORIENTED_EDGE('',*,*,#959,.F.);
#1263=ORIENTED_EDGE('',*,*,#960,.F.);
#1264=ORIENTED_EDGE('',*,*,#961,.T.);
#1265=ORIENTED_EDGE('',*,*,#962,.T.);
#1266=ORIENTED_EDGE('',*,*,#961,.F.);
#1267=ORIENTED_EDGE('',*,*,#963,.F.);
#1268=ORIENTED_EDGE('',*,*,#960,.T.);
#1269=ORIENTED_EDGE('',*,*,#964,.F.);
#1270=ORIENTED_EDGE('',*,*,#965,.T.);
#1271=ORIENTED_EDGE('',*,*,#963,.T.);
#1272=ORIENTED_EDGE('',*,*,#965,.F.);
#1273=ORIENTED_EDGE('',*,*,#964,.T.);
#1274=ORIENTED_EDGE('',*,*,#966,.F.);
#1275=ORIENTED_EDGE('',*,*,#967,.F.);
#1276=ORIENTED_EDGE('',*,*,#968,.T.);
#1277=ORIENTED_EDGE('',*,*,#966,.T.);
#1278=ORIENTED_EDGE('',*,*,#968,.F.);
#1279=ORIENTED_EDGE('',*,*,#967,.T.);
#1280=ORIENTED_EDGE('',*,*,#962,.F.);
#1281=ORIENTED_EDGE('',*,*,#969,.F.);
#1282=ORIENTED_EDGE('',*,*,#970,.F.);
#1283=ORIENTED_EDGE('',*,*,#971,.F.);
#1284=ORIENTED_EDGE('',*,*,#972,.T.);
#1285=ORIENTED_EDGE('',*,*,#973,.F.);
#1286=ORIENTED_EDGE('',*,*,#974,.F.);
#1287=ORIENTED_EDGE('',*,*,#975,.F.);
#1288=ORIENTED_EDGE('',*,*,#969,.T.);
#1289=ORIENTED_EDGE('',*,*,#976,.T.);
#1290=ORIENTED_EDGE('',*,*,#977,.T.);
#1291=ORIENTED_EDGE('',*,*,#978,.F.);
#1292=ORIENTED_EDGE('',*,*,#979,.F.);
#1293=ORIENTED_EDGE('',*,*,#973,.T.);
#1294=ORIENTED_EDGE('',*,*,#980,.T.);
#1295=ORIENTED_EDGE('',*,*,#981,.T.);
#1296=ORIENTED_EDGE('',*,*,#982,.F.);
#1297=ORIENTED_EDGE('',*,*,#983,.F.);
#1298=ORIENTED_EDGE('',*,*,#984,.F.);
#1299=ORIENTED_EDGE('',*,*,#978,.T.);
#1300=ORIENTED_EDGE('',*,*,#985,.T.);
#1301=ORIENTED_EDGE('',*,*,#986,.F.);
#1302=ORIENTED_EDGE('',*,*,#987,.F.);
#1303=ORIENTED_EDGE('',*,*,#982,.T.);
#1304=ORIENTED_EDGE('',*,*,#988,.T.);
#1305=ORIENTED_EDGE('',*,*,#989,.T.);
#1306=ORIENTED_EDGE('',*,*,#990,.F.);
#1307=ORIENTED_EDGE('',*,*,#991,.F.);
#1308=ORIENTED_EDGE('',*,*,#992,.F.);
#1309=ORIENTED_EDGE('',*,*,#986,.T.);
#1310=ORIENTED_EDGE('',*,*,#993,.T.);
#1311=ORIENTED_EDGE('',*,*,#994,.F.);
#1312=ORIENTED_EDGE('',*,*,#995,.F.);
#1313=ORIENTED_EDGE('',*,*,#990,.T.);
#1314=ORIENTED_EDGE('',*,*,#996,.T.);
#1315=ORIENTED_EDGE('',*,*,#997,.T.);
#1316=ORIENTED_EDGE('',*,*,#998,.F.);
#1317=ORIENTED_EDGE('',*,*,#999,.F.);
#1318=ORIENTED_EDGE('',*,*,#1000,.F.);
#1319=ORIENTED_EDGE('',*,*,#994,.T.);
#1320=ORIENTED_EDGE('',*,*,#1001,.T.);
#1321=ORIENTED_EDGE('',*,*,#1002,.F.);
#1322=ORIENTED_EDGE('',*,*,#1003,.F.);
#1323=ORIENTED_EDGE('',*,*,#998,.T.);
#1324=ORIENTED_EDGE('',*,*,#1004,.T.);
#1325=ORIENTED_EDGE('',*,*,#1005,.T.);
#1326=ORIENTED_EDGE('',*,*,#1006,.F.);
#1327=ORIENTED_EDGE('',*,*,#1007,.F.);
#1328=ORIENTED_EDGE('',*,*,#1008,.F.);
#1329=ORIENTED_EDGE('',*,*,#1002,.T.);
#1330=ORIENTED_EDGE('',*,*,#1009,.T.);
#1331=ORIENTED_EDGE('',*,*,#1010,.F.);
#1332=ORIENTED_EDGE('',*,*,#1011,.F.);
#1333=ORIENTED_EDGE('',*,*,#1006,.T.);
#1334=ORIENTED_EDGE('',*,*,#1012,.T.);
#1335=ORIENTED_EDGE('',*,*,#1013,.T.);
#1336=ORIENTED_EDGE('',*,*,#1014,.T.);
#1337=ORIENTED_EDGE('',*,*,#1015,.T.);
#1338=ORIENTED_EDGE('',*,*,#1016,.T.);
#1339=ORIENTED_EDGE('',*,*,#1017,.T.);
#1340=ORIENTED_EDGE('',*,*,#1018,.T.);
#1341=ORIENTED_EDGE('',*,*,#1019,.T.);
#1342=ORIENTED_EDGE('',*,*,#1020,.T.);
#1343=ORIENTED_EDGE('',*,*,#1021,.T.);
#1344=ORIENTED_EDGE('',*,*,#1022,.T.);
#1345=ORIENTED_EDGE('',*,*,#1023,.T.);
#1346=ORIENTED_EDGE('',*,*,#1024,.T.);
#1347=ORIENTED_EDGE('',*,*,#1025,.T.);
#1348=ORIENTED_EDGE('',*,*,#1026,.T.);
#1349=ORIENTED_EDGE('',*,*,#1027,.T.);
#1350=ORIENTED_EDGE('',*,*,#1028,.T.);
#1351=ORIENTED_EDGE('',*,*,#1029,.F.);
#1352=ORIENTED_EDGE('',*,*,#1030,.T.);
#1353=ORIENTED_EDGE('',*,*,#1031,.T.);
#1354=ORIENTED_EDGE('',*,*,#1032,.T.);
#1355=ORIENTED_EDGE('',*,*,#1033,.T.);
#1356=ORIENTED_EDGE('',*,*,#1034,.T.);
#1357=ORIENTED_EDGE('',*,*,#1035,.T.);
#1358=ORIENTED_EDGE('',*,*,#1036,.T.);
#1359=ORIENTED_EDGE('',*,*,#1037,.T.);
#1360=ORIENTED_EDGE('',*,*,#1038,.T.);
#1361=ORIENTED_EDGE('',*,*,#1039,.T.);
#1362=ORIENTED_EDGE('',*,*,#1040,.T.);
#1363=ORIENTED_EDGE('',*,*,#1041,.T.);
#1364=ORIENTED_EDGE('',*,*,#1010,.T.);
#1365=ORIENTED_EDGE('',*,*,#1042,.T.);
#1366=ORIENTED_EDGE('',*,*,#1043,.F.);
#1367=ORIENTED_EDGE('',*,*,#1044,.F.);
#1368=ORIENTED_EDGE('',*,*,#1045,.F.);
#1369=ORIENTED_EDGE('',*,*,#1046,.F.);
#1370=ORIENTED_EDGE('',*,*,#1028,.F.);
#1371=ORIENTED_EDGE('',*,*,#1027,.F.);
#1372=ORIENTED_EDGE('',*,*,#1026,.F.);
#1373=ORIENTED_EDGE('',*,*,#1025,.F.);
#1374=ORIENTED_EDGE('',*,*,#1024,.F.);
#1375=ORIENTED_EDGE('',*,*,#1023,.F.);
#1376=ORIENTED_EDGE('',*,*,#1022,.F.);
#1377=ORIENTED_EDGE('',*,*,#1021,.F.);
#1378=ORIENTED_EDGE('',*,*,#1020,.F.);
#1379=ORIENTED_EDGE('',*,*,#1019,.F.);
#1380=ORIENTED_EDGE('',*,*,#1018,.F.);
#1381=ORIENTED_EDGE('',*,*,#1017,.F.);
#1382=ORIENTED_EDGE('',*,*,#1016,.F.);
#1383=ORIENTED_EDGE('',*,*,#1047,.F.);
#1384=ORIENTED_EDGE('',*,*,#970,.T.);
#1385=ORIENTED_EDGE('',*,*,#975,.T.);
#1386=ORIENTED_EDGE('',*,*,#974,.T.);
#1387=ORIENTED_EDGE('',*,*,#979,.T.);
#1388=ORIENTED_EDGE('',*,*,#984,.T.);
#1389=ORIENTED_EDGE('',*,*,#983,.T.);
#1390=ORIENTED_EDGE('',*,*,#987,.T.);
#1391=ORIENTED_EDGE('',*,*,#992,.T.);
#1392=ORIENTED_EDGE('',*,*,#991,.T.);
#1393=ORIENTED_EDGE('',*,*,#995,.T.);
#1394=ORIENTED_EDGE('',*,*,#1000,.T.);
#1395=ORIENTED_EDGE('',*,*,#999,.T.);
#1396=ORIENTED_EDGE('',*,*,#1003,.T.);
#1397=ORIENTED_EDGE('',*,*,#1008,.T.);
#1398=ORIENTED_EDGE('',*,*,#1007,.T.);
#1399=ORIENTED_EDGE('',*,*,#1011,.T.);
#1400=ORIENTED_EDGE('',*,*,#1045,.T.);
#1401=ORIENTED_EDGE('',*,*,#1044,.T.);
#1402=ORIENTED_EDGE('',*,*,#1048,.F.);
#1403=ORIENTED_EDGE('',*,*,#1049,.F.);
#1404=ORIENTED_EDGE('',*,*,#1042,.F.);
#1405=ORIENTED_EDGE('',*,*,#1013,.F.);
#1406=ORIENTED_EDGE('',*,*,#1012,.F.);
#1407=ORIENTED_EDGE('',*,*,#1009,.F.);
#1408=ORIENTED_EDGE('',*,*,#1005,.F.);
#1409=ORIENTED_EDGE('',*,*,#1004,.F.);
#1410=ORIENTED_EDGE('',*,*,#1001,.F.);
#1411=ORIENTED_EDGE('',*,*,#997,.F.);
#1412=ORIENTED_EDGE('',*,*,#996,.F.);
#1413=ORIENTED_EDGE('',*,*,#993,.F.);
#1414=ORIENTED_EDGE('',*,*,#989,.F.);
#1415=ORIENTED_EDGE('',*,*,#988,.F.);
#1416=ORIENTED_EDGE('',*,*,#985,.F.);
#1417=ORIENTED_EDGE('',*,*,#981,.F.);
#1418=ORIENTED_EDGE('',*,*,#980,.F.);
#1419=ORIENTED_EDGE('',*,*,#977,.F.);
#1420=ORIENTED_EDGE('',*,*,#976,.F.);
#1421=ORIENTED_EDGE('',*,*,#972,.F.);
#1422=ORIENTED_EDGE('',*,*,#1050,.F.);
#1423=ORIENTED_EDGE('',*,*,#1014,.F.);
#1424=ORIENTED_EDGE('',*,*,#1041,.F.);
#1425=ORIENTED_EDGE('',*,*,#1040,.F.);
#1426=ORIENTED_EDGE('',*,*,#1039,.F.);
#1427=ORIENTED_EDGE('',*,*,#1038,.F.);
#1428=ORIENTED_EDGE('',*,*,#1037,.F.);
#1429=ORIENTED_EDGE('',*,*,#1036,.F.);
#1430=ORIENTED_EDGE('',*,*,#1035,.F.);
#1431=ORIENTED_EDGE('',*,*,#1034,.F.);
#1432=ORIENTED_EDGE('',*,*,#1033,.F.);
#1433=ORIENTED_EDGE('',*,*,#1032,.F.);
#1434=ORIENTED_EDGE('',*,*,#1031,.F.);
#1435=ORIENTED_EDGE('',*,*,#1030,.F.);
#1436=ORIENTED_EDGE('',*,*,#1051,.T.);
#1437=ORIENTED_EDGE('',*,*,#1047,.T.);
#1438=ORIENTED_EDGE('',*,*,#1015,.F.);
#1439=ORIENTED_EDGE('',*,*,#1050,.T.);
#1440=ORIENTED_EDGE('',*,*,#971,.T.);
#1441=ORIENTED_EDGE('',*,*,#1052,.F.);
#1442=ORIENTED_EDGE('',*,*,#1029,.T.);
#1443=ORIENTED_EDGE('',*,*,#1046,.T.);
#1444=ORIENTED_EDGE('',*,*,#1043,.T.);
#1445=ORIENTED_EDGE('',*,*,#1049,.T.);
#1446=ORIENTED_EDGE('',*,*,#1048,.T.);
#1447=ORIENTED_EDGE('',*,*,#1053,.F.);
#1448=ORIENTED_EDGE('',*,*,#1054,.T.);
#1449=ORIENTED_EDGE('',*,*,#1052,.T.);
#1450=ORIENTED_EDGE('',*,*,#1054,.F.);
#1451=ORIENTED_EDGE('',*,*,#1053,.T.);
#1452=ORIENTED_EDGE('',*,*,#1055,.T.);
#1453=ORIENTED_EDGE('',*,*,#1056,.F.);
#1454=ORIENTED_EDGE('',*,*,#1055,.F.);
#1455=ORIENTED_EDGE('',*,*,#1057,.F.);
#1456=ORIENTED_EDGE('',*,*,#1058,.T.);
#1457=ORIENTED_EDGE('',*,*,#1056,.T.);
#1458=ORIENTED_EDGE('',*,*,#1058,.F.);
#1459=ORIENTED_EDGE('',*,*,#1059,.F.);
#1460=ORIENTED_EDGE('',*,*,#1057,.T.);
#1461=ORIENTED_EDGE('',*,*,#1060,.F.);
#1462=ORIENTED_EDGE('',*,*,#1061,.T.);
#1463=ORIENTED_EDGE('',*,*,#1059,.T.);
#1464=ORIENTED_EDGE('',*,*,#1061,.F.);
#1465=ORIENTED_EDGE('',*,*,#1062,.F.);
#1466=ORIENTED_EDGE('',*,*,#1063,.T.);
#1467=ORIENTED_EDGE('',*,*,#1060,.T.);
#1468=ORIENTED_EDGE('',*,*,#1063,.F.);
#1469=ORIENTED_EDGE('',*,*,#1062,.T.);
#1470=ORIENTED_EDGE('',*,*,#1064,.F.);
#1471=ORIENTED_EDGE('',*,*,#1065,.F.);
#1472=ORIENTED_EDGE('',*,*,#1066,.T.);
#1473=ORIENTED_EDGE('',*,*,#1064,.T.);
#1474=ORIENTED_EDGE('',*,*,#1066,.F.);
#1475=ORIENTED_EDGE('',*,*,#1067,.F.);
#1476=ORIENTED_EDGE('',*,*,#1065,.T.);
#1477=ORIENTED_EDGE('',*,*,#1051,.F.);
#1478=ORIENTED_EDGE('',*,*,#1068,.T.);
#1479=ORIENTED_EDGE('',*,*,#1067,.T.);
#1480=ORIENTED_EDGE('',*,*,#1068,.F.);
#1481=ORIENTED_EDGE('',*,*,#1069,.F.);
#1482=ORIENTED_EDGE('',*,*,#1070,.T.);
#1483=ORIENTED_EDGE('',*,*,#1069,.T.);
#1484=ORIENTED_EDGE('',*,*,#1071,.T.);
#1485=ORIENTED_EDGE('',*,*,#1072,.F.);
#1486=ORIENTED_EDGE('',*,*,#1071,.F.);
#1487=ORIENTED_EDGE('',*,*,#1073,.F.);
#1488=ORIENTED_EDGE('',*,*,#1072,.T.);
#1489=ORIENTED_EDGE('',*,*,#1074,.F.);
#1490=ORIENTED_EDGE('',*,*,#1075,.T.);
#1491=ORIENTED_EDGE('',*,*,#1073,.T.);
#1492=ORIENTED_EDGE('',*,*,#1075,.F.);
#1493=ORIENTED_EDGE('',*,*,#1076,.F.);
#1494=ORIENTED_EDGE('',*,*,#1074,.T.);
#1495=ORIENTED_EDGE('',*,*,#1077,.F.);
#1496=ORIENTED_EDGE('',*,*,#1078,.T.);
#1497=ORIENTED_EDGE('',*,*,#1076,.T.);
#1498=ORIENTED_EDGE('',*,*,#1078,.F.);
#1499=ORIENTED_EDGE('',*,*,#1077,.T.);
#1500=ORIENTED_EDGE('',*,*,#1079,.T.);
#1501=ORIENTED_EDGE('',*,*,#1080,.F.);
#1502=ORIENTED_EDGE('',*,*,#1079,.F.);
#1503=ORIENTED_EDGE('',*,*,#1080,.T.);
#1504=ORIENTED_EDGE('',*,*,#1081,.F.);
#1505=ORIENTED_EDGE('',*,*,#1081,.T.);
#1506=ORIENTED_EDGE('',*,*,#1082,.T.);
#1507=ORIENTED_EDGE('',*,*,#1083,.F.);
#1508=ORIENTED_EDGE('',*,*,#1082,.F.);
#1509=ORIENTED_EDGE('',*,*,#1083,.T.);
#1510=ORIENTED_EDGE('',*,*,#1084,.F.);
#1511=ORIENTED_EDGE('',*,*,#1085,.F.);
#1512=ORIENTED_EDGE('',*,*,#1086,.T.);
#1513=ORIENTED_EDGE('',*,*,#1084,.T.);
#1514=ORIENTED_EDGE('',*,*,#1086,.F.);
#1515=ORIENTED_EDGE('',*,*,#1085,.T.);
#1516=ORIENTED_EDGE('',*,*,#1087,.F.);
#1517=ORIENTED_EDGE('',*,*,#1088,.F.);
#1518=ORIENTED_EDGE('',*,*,#1089,.T.);
#1519=ORIENTED_EDGE('',*,*,#1087,.T.);
#1520=ORIENTED_EDGE('',*,*,#1089,.F.);
#1521=ORIENTED_EDGE('',*,*,#1088,.T.);
#1522=ORIENTED_EDGE('',*,*,#1090,.F.);
#1523=ORIENTED_EDGE('',*,*,#1091,.F.);
#1524=ORIENTED_EDGE('',*,*,#1092,.T.);
#1525=ORIENTED_EDGE('',*,*,#1090,.T.);
#1526=ORIENTED_EDGE('',*,*,#1092,.F.);
#1527=ORIENTED_EDGE('',*,*,#1091,.T.);
#1528=ORIENTED_EDGE('',*,*,#1093,.F.);
#1529=ORIENTED_EDGE('',*,*,#1094,.F.);
#1530=ORIENTED_EDGE('',*,*,#1095,.T.);
#1531=ORIENTED_EDGE('',*,*,#1093,.T.);
#1532=ORIENTED_EDGE('',*,*,#1095,.F.);
#1533=ORIENTED_EDGE('',*,*,#1096,.F.);
#1534=ORIENTED_EDGE('',*,*,#1097,.T.);
#1535=ORIENTED_EDGE('',*,*,#1094,.T.);
#1536=ORIENTED_EDGE('',*,*,#1097,.F.);
#1537=ORIENTED_EDGE('',*,*,#1070,.F.);
#1538=ORIENTED_EDGE('',*,*,#1098,.T.);
#1539=ORIENTED_EDGE('',*,*,#1096,.T.);
#1540=ORIENTED_EDGE('',*,*,#1098,.F.);
#1541=ORIENTED_EDGE('',*,*,#1099,.F.);
#1542=ORIENTED_EDGE('',*,*,#1100,.F.);
#1543=ORIENTED_EDGE('',*,*,#1101,.F.);
#1544=ORIENTED_EDGE('',*,*,#1102,.T.);
#1545=ORIENTED_EDGE('',*,*,#1103,.F.);
#1546=ORIENTED_EDGE('',*,*,#1104,.F.);
#1547=ORIENTED_EDGE('',*,*,#1105,.F.);
#1548=ORIENTED_EDGE('',*,*,#1099,.T.);
#1549=ORIENTED_EDGE('',*,*,#1106,.T.);
#1550=ORIENTED_EDGE('',*,*,#1107,.F.);
#1551=ORIENTED_EDGE('',*,*,#1108,.F.);
#1552=ORIENTED_EDGE('',*,*,#1109,.F.);
#1553=ORIENTED_EDGE('',*,*,#1103,.T.);
#1554=ORIENTED_EDGE('',*,*,#1110,.T.);
#1555=ORIENTED_EDGE('',*,*,#1111,.T.);
#1556=ORIENTED_EDGE('',*,*,#1112,.F.);
#1557=ORIENTED_EDGE('',*,*,#1113,.F.);
#1558=ORIENTED_EDGE('',*,*,#1107,.T.);
#1559=ORIENTED_EDGE('',*,*,#1114,.T.);
#1560=ORIENTED_EDGE('',*,*,#1115,.F.);
#1561=ORIENTED_EDGE('',*,*,#1116,.F.);
#1562=ORIENTED_EDGE('',*,*,#1117,.F.);
#1563=ORIENTED_EDGE('',*,*,#1112,.T.);
#1564=ORIENTED_EDGE('',*,*,#1118,.T.);
#1565=ORIENTED_EDGE('',*,*,#1119,.T.);
#1566=ORIENTED_EDGE('',*,*,#1120,.F.);
#1567=ORIENTED_EDGE('',*,*,#1121,.F.);
#1568=ORIENTED_EDGE('',*,*,#1115,.T.);
#1569=ORIENTED_EDGE('',*,*,#1122,.T.);
#1570=ORIENTED_EDGE('',*,*,#1123,.F.);
#1571=ORIENTED_EDGE('',*,*,#1124,.F.);
#1572=ORIENTED_EDGE('',*,*,#1125,.F.);
#1573=ORIENTED_EDGE('',*,*,#1120,.T.);
#1574=ORIENTED_EDGE('',*,*,#1126,.T.);
#1575=ORIENTED_EDGE('',*,*,#1127,.T.);
#1576=ORIENTED_EDGE('',*,*,#1128,.T.);
#1577=ORIENTED_EDGE('',*,*,#1129,.T.);
#1578=ORIENTED_EDGE('',*,*,#1130,.T.);
#1579=ORIENTED_EDGE('',*,*,#1131,.T.);
#1580=ORIENTED_EDGE('',*,*,#1132,.T.);
#1581=ORIENTED_EDGE('',*,*,#1133,.T.);
#1582=ORIENTED_EDGE('',*,*,#1134,.T.);
#1583=ORIENTED_EDGE('',*,*,#1135,.T.);
#1584=ORIENTED_EDGE('',*,*,#1136,.T.);
#1585=ORIENTED_EDGE('',*,*,#1137,.T.);
#1586=ORIENTED_EDGE('',*,*,#1138,.T.);
#1587=ORIENTED_EDGE('',*,*,#1139,.F.);
#1588=ORIENTED_EDGE('',*,*,#1140,.T.);
#1589=ORIENTED_EDGE('',*,*,#1141,.T.);
#1590=ORIENTED_EDGE('',*,*,#1142,.T.);
#1591=ORIENTED_EDGE('',*,*,#1143,.T.);
#1592=ORIENTED_EDGE('',*,*,#1144,.T.);
#1593=ORIENTED_EDGE('',*,*,#1145,.T.);
#1594=ORIENTED_EDGE('',*,*,#1146,.T.);
#1595=ORIENTED_EDGE('',*,*,#1147,.T.);
#1596=ORIENTED_EDGE('',*,*,#1123,.T.);
#1597=ORIENTED_EDGE('',*,*,#1148,.T.);
#1598=ORIENTED_EDGE('',*,*,#1149,.F.);
#1599=ORIENTED_EDGE('',*,*,#1150,.F.);
#1600=ORIENTED_EDGE('',*,*,#1151,.F.);
#1601=ORIENTED_EDGE('',*,*,#1138,.F.);
#1602=ORIENTED_EDGE('',*,*,#1137,.F.);
#1603=ORIENTED_EDGE('',*,*,#1136,.F.);
#1604=ORIENTED_EDGE('',*,*,#1135,.F.);
#1605=ORIENTED_EDGE('',*,*,#1134,.F.);
#1606=ORIENTED_EDGE('',*,*,#1133,.F.);
#1607=ORIENTED_EDGE('',*,*,#1132,.F.);
#1608=ORIENTED_EDGE('',*,*,#1131,.F.);
#1609=ORIENTED_EDGE('',*,*,#1130,.F.);
#1610=ORIENTED_EDGE('',*,*,#1152,.F.);
#1611=ORIENTED_EDGE('',*,*,#1100,.T.);
#1612=ORIENTED_EDGE('',*,*,#1105,.T.);
#1613=ORIENTED_EDGE('',*,*,#1104,.T.);
#1614=ORIENTED_EDGE('',*,*,#1109,.T.);
#1615=ORIENTED_EDGE('',*,*,#1108,.T.);
#1616=ORIENTED_EDGE('',*,*,#1113,.T.);
#1617=ORIENTED_EDGE('',*,*,#1117,.T.);
#1618=ORIENTED_EDGE('',*,*,#1116,.T.);
#1619=ORIENTED_EDGE('',*,*,#1121,.T.);
#1620=ORIENTED_EDGE('',*,*,#1125,.T.);
#1621=ORIENTED_EDGE('',*,*,#1124,.T.);
#1622=ORIENTED_EDGE('',*,*,#1150,.T.);
#1623=ORIENTED_EDGE('',*,*,#1153,.T.);
#1624=ORIENTED_EDGE('',*,*,#1154,.T.);
#1625=ORIENTED_EDGE('',*,*,#1155,.T.);
#1626=ORIENTED_EDGE('',*,*,#1101,.T.);
#1627=ORIENTED_EDGE('',*,*,#1152,.T.);
#1628=ORIENTED_EDGE('',*,*,#1156,.F.);
#1629=ORIENTED_EDGE('',*,*,#1157,.F.);
#1630=ORIENTED_EDGE('',*,*,#1148,.F.);
#1631=ORIENTED_EDGE('',*,*,#1127,.F.);
#1632=ORIENTED_EDGE('',*,*,#1126,.F.);
#1633=ORIENTED_EDGE('',*,*,#1122,.F.);
#1634=ORIENTED_EDGE('',*,*,#1119,.F.);
#1635=ORIENTED_EDGE('',*,*,#1118,.F.);
#1636=ORIENTED_EDGE('',*,*,#1114,.F.);
#1637=ORIENTED_EDGE('',*,*,#1111,.F.);
#1638=ORIENTED_EDGE('',*,*,#1110,.F.);
#1639=ORIENTED_EDGE('',*,*,#1106,.F.);
#1640=ORIENTED_EDGE('',*,*,#1102,.F.);
#1641=ORIENTED_EDGE('',*,*,#1155,.F.);
#1642=ORIENTED_EDGE('',*,*,#1158,.T.);
#1643=ORIENTED_EDGE('',*,*,#1128,.F.);
#1644=ORIENTED_EDGE('',*,*,#1147,.F.);
#1645=ORIENTED_EDGE('',*,*,#1146,.F.);
#1646=ORIENTED_EDGE('',*,*,#1145,.F.);
#1647=ORIENTED_EDGE('',*,*,#1144,.F.);
#1648=ORIENTED_EDGE('',*,*,#1143,.F.);
#1649=ORIENTED_EDGE('',*,*,#1142,.F.);
#1650=ORIENTED_EDGE('',*,*,#1141,.F.);
#1651=ORIENTED_EDGE('',*,*,#1140,.F.);
#1652=ORIENTED_EDGE('',*,*,#1158,.F.);
#1653=ORIENTED_EDGE('',*,*,#1154,.F.);
#1654=ORIENTED_EDGE('',*,*,#1159,.T.);
#1655=ORIENTED_EDGE('',*,*,#1160,.T.);
#1656=ORIENTED_EDGE('',*,*,#1159,.F.);
#1657=ORIENTED_EDGE('',*,*,#1153,.F.);
#1658=ORIENTED_EDGE('',*,*,#1129,.F.);
#1659=ORIENTED_EDGE('',*,*,#1161,.F.);
#1660=ORIENTED_EDGE('',*,*,#1139,.T.);
#1661=ORIENTED_EDGE('',*,*,#1151,.T.);
#1662=ORIENTED_EDGE('',*,*,#1149,.T.);
#1663=ORIENTED_EDGE('',*,*,#1157,.T.);
#1664=ORIENTED_EDGE('',*,*,#1156,.T.);
#1665=ORIENTED_EDGE('',*,*,#1162,.F.);
#1666=ORIENTED_EDGE('',*,*,#1163,.T.);
#1667=ORIENTED_EDGE('',*,*,#1161,.T.);
#1668=ORIENTED_EDGE('',*,*,#1163,.F.);
#1669=ORIENTED_EDGE('',*,*,#1162,.T.);
#1670=ORIENTED_EDGE('',*,*,#1164,.T.);
#1671=ORIENTED_EDGE('',*,*,#1165,.F.);
#1672=ORIENTED_EDGE('',*,*,#1164,.F.);
#1673=ORIENTED_EDGE('',*,*,#1165,.T.);
#1674=ORIENTED_EDGE('',*,*,#1166,.F.);
#1675=ORIENTED_EDGE('',*,*,#1167,.F.);
#1676=ORIENTED_EDGE('',*,*,#1168,.T.);
#1677=ORIENTED_EDGE('',*,*,#1166,.T.);
#1678=ORIENTED_EDGE('',*,*,#1168,.F.);
#1679=ORIENTED_EDGE('',*,*,#1167,.T.);
#1680=ORIENTED_EDGE('',*,*,#1169,.F.);
#1681=ORIENTED_EDGE('',*,*,#1160,.F.);
#1682=ORIENTED_EDGE('',*,*,#1170,.T.);
#1683=ORIENTED_EDGE('',*,*,#1169,.T.);
#1684=ORIENTED_EDGE('',*,*,#1170,.F.);
#1685=PLANE('',#1925);
#1686=PLANE('',#1928);
#1687=PLANE('',#1934);
#1688=PLANE('',#1939);
#1689=PLANE('',#1943);
#1690=PLANE('',#1947);
#1691=PLANE('',#1954);
#1692=PLANE('',#1958);
#1693=PLANE('',#1962);
#1694=PLANE('',#1963);
#1695=PLANE('',#1970);
#1696=PLANE('',#1974);
#1697=PLANE('',#1983);
#1698=PLANE('',#1988);
#1699=PLANE('',#1995);
#1700=PLANE('',#1999);
#1701=PLANE('',#2003);
#1702=PLANE('',#2022);
#1703=PLANE('',#2024);
#1704=PLANE('',#2025);
#1705=PLANE('',#2033);
#1706=PLANE('',#2040);
#1707=PLANE('',#2044);
#1708=PLANE('',#2048);
#1709=PLANE('',#2053);
#1710=PLANE('',#2057);
#1711=PLANE('',#2063);
#1712=PLANE('',#2067);
#1713=PLANE('',#2071);
#1714=PLANE('',#2075);
#1715=PLANE('',#2079);
#1716=PLANE('',#2100);
#1717=PLANE('',#2106);
#1718=PLANE('',#2112);
#1719=PLANE('',#2116);
#1720=PLANE('',#2117);
#1721=ADVANCED_FACE('',(#399,#370),#1685,.T.);
#1722=ADVANCED_FACE('',(#400,#371),#1686,.T.);
#1723=ADVANCED_FACE('',(#401),#318,.F.);
#1724=ADVANCED_FACE('',(#402),#319,.T.);
#1725=ADVANCED_FACE('',(#403),#1687,.T.);
#1726=ADVANCED_FACE('',(#404),#320,.T.);
#1727=ADVANCED_FACE('',(#405,#372),#1688,.T.);
#1728=ADVANCED_FACE('',(#406),#321,.F.);
#1729=ADVANCED_FACE('',(#407,#373),#1689,.T.);
#1730=ADVANCED_FACE('',(#408),#322,.T.);
#1731=ADVANCED_FACE('',(#409,#374),#1690,.T.);
#1732=ADVANCED_FACE('',(#410),#323,.T.);
#1733=ADVANCED_FACE('',(#411),#171,.T.);
#1734=ADVANCED_FACE('',(#412,#375),#1691,.T.);
#1735=ADVANCED_FACE('',(#413),#324,.F.);
#1736=ADVANCED_FACE('',(#414,#376),#1692,.T.);
#1737=ADVANCED_FACE('',(#415),#325,.F.);
#1738=ADVANCED_FACE('',(#416),#1693,.T.);
#1739=ADVANCED_FACE('',(#417,#377),#1694,.F.);
#1740=ADVANCED_FACE('',(#418),#326,.F.);
#1741=ADVANCED_FACE('',(#419),#327,.T.);
#1742=ADVANCED_FACE('',(#420,#378),#1695,.T.);
#1743=ADVANCED_FACE('',(#421),#328,.T.);
#1744=ADVANCED_FACE('',(#422,#379),#1696,.T.);
#1745=ADVANCED_FACE('',(#423),#329,.T.);
#1746=ADVANCED_FACE('',(#424),#169,.T.);
#1747=ADVANCED_FACE('',(#425),#170,.T.);
#1748=ADVANCED_FACE('',(#426,#380),#1697,.F.);
#1749=ADVANCED_FACE('',(#427),#330,.T.);
#1750=ADVANCED_FACE('',(#428,#381),#1698,.T.);
#1751=ADVANCED_FACE('',(#429),#331,.F.);
#1752=ADVANCED_FACE('',(#430),#332,.F.);
#1753=ADVANCED_FACE('',(#431,#382),#1699,.T.);
#1754=ADVANCED_FACE('',(#432),#333,.T.);
#1755=ADVANCED_FACE('',(#433,#383),#1700,.T.);
#1756=ADVANCED_FACE('',(#434),#334,.F.);
#1757=ADVANCED_FACE('',(#435,#384),#1701,.T.);
#1758=ADVANCED_FACE('',(#436),#335,.T.);
#1759=ADVANCED_FACE('',(#437),#336,.T.);
#1760=ADVANCED_FACE('',(#438),#337,.T.);
#1761=ADVANCED_FACE('',(#439),#338,.T.);
#1762=ADVANCED_FACE('',(#440),#339,.T.);
#1763=ADVANCED_FACE('',(#441),#340,.T.);
#1764=ADVANCED_FACE('',(#442),#341,.T.);
#1765=ADVANCED_FACE('',(#443),#342,.T.);
#1766=ADVANCED_FACE('',(#444),#343,.T.);
#1767=ADVANCED_FACE('',(#445),#344,.T.);
#1768=ADVANCED_FACE('',(#446),#345,.T.);
#1769=ADVANCED_FACE('',(#447),#346,.T.);
#1770=ADVANCED_FACE('',(#448),#347,.T.);
#1771=ADVANCED_FACE('',(#449),#51,.F.);
#1772=ADVANCED_FACE('',(#450),#52,.F.);
#1773=ADVANCED_FACE('',(#451),#1702,.T.);
#1774=ADVANCED_FACE('',(#452),#1703,.T.);
#1775=ADVANCED_FACE('',(#453,#385),#1704,.T.);
#1776=ADVANCED_FACE('',(#454),#348,.T.);
#1777=ADVANCED_FACE('',(#455),#43,.T.);
#1778=ADVANCED_FACE('',(#456),#349,.T.);
#1779=ADVANCED_FACE('',(#457,#386),#1705,.T.);
#1780=ADVANCED_FACE('',(#458),#350,.T.);
#1781=ADVANCED_FACE('',(#459),#172,.T.);
#1782=ADVANCED_FACE('',(#460,#387),#1706,.T.);
#1783=ADVANCED_FACE('',(#461),#351,.F.);
#1784=ADVANCED_FACE('',(#462,#388),#1707,.T.);
#1785=ADVANCED_FACE('',(#463),#352,.F.);
#1786=ADVANCED_FACE('',(#464,#389),#1708,.T.);
#1787=ADVANCED_FACE('',(#465),#44,.F.);
#1788=ADVANCED_FACE('',(#466,#390),#1709,.T.);
#1789=ADVANCED_FACE('',(#467),#45,.T.);
#1790=ADVANCED_FACE('',(#468,#391),#1710,.T.);
#1791=ADVANCED_FACE('',(#469),#353,.T.);
#1792=ADVANCED_FACE('',(#470),#46,.T.);
#1793=ADVANCED_FACE('',(#471,#392),#1711,.T.);
#1794=ADVANCED_FACE('',(#472),#47,.T.);
#1795=ADVANCED_FACE('',(#473,#393),#1712,.T.);
#1796=ADVANCED_FACE('',(#474),#354,.T.);
#1797=ADVANCED_FACE('',(#475,#394),#1713,.T.);
#1798=ADVANCED_FACE('',(#476),#48,.F.);
#1799=ADVANCED_FACE('',(#477,#395),#1714,.T.);
#1800=ADVANCED_FACE('',(#478),#355,.F.);
#1801=ADVANCED_FACE('',(#479,#396),#1715,.T.);
#1802=ADVANCED_FACE('',(#480),#356,.F.);
#1803=ADVANCED_FACE('',(#481),#49,.F.);
#1804=ADVANCED_FACE('',(#482),#357,.F.);
#1805=ADVANCED_FACE('',(#483),#358,.T.);
#1806=ADVANCED_FACE('',(#484),#359,.T.);
#1807=ADVANCED_FACE('',(#485),#360,.T.);
#1808=ADVANCED_FACE('',(#486),#361,.T.);
#1809=ADVANCED_FACE('',(#487),#362,.T.);
#1810=ADVANCED_FACE('',(#488),#363,.T.);
#1811=ADVANCED_FACE('',(#489),#364,.T.);
#1812=ADVANCED_FACE('',(#490),#365,.T.);
#1813=ADVANCED_FACE('',(#491),#366,.T.);
#1814=ADVANCED_FACE('',(#492),#53,.F.);
#1815=ADVANCED_FACE('',(#493),#1716,.T.);
#1816=ADVANCED_FACE('',(#494),#54,.F.);
#1817=ADVANCED_FACE('',(#495),#173,.F.);
#1818=ADVANCED_FACE('',(#496,#397),#1717,.T.);
#1819=ADVANCED_FACE('',(#497),#367,.T.);
#1820=ADVANCED_FACE('',(#498),#50,.T.);
#1821=ADVANCED_FACE('',(#499,#398),#1718,.T.);
#1822=ADVANCED_FACE('',(#500),#368,.F.);
#1823=ADVANCED_FACE('',(#501),#1719,.T.);
#1824=ADVANCED_FACE('',(#502),#1720,.T.);
#1825=ADVANCED_FACE('',(#503),#369,.T.);
#1826=CLOSED_SHELL('',(#1721,#1722,#1723,#1724));
#1827=CLOSED_SHELL('',(#1725,#1726,#1727,#1728,#1729,#1730,#1731,#1732,
#1733,#1734,#1735,#1736,#1737,#1738,#1739,#1740));
#1828=CLOSED_SHELL('',(#1741,#1742,#1743,#1744,#1745,#1746,#1747));
#1829=CLOSED_SHELL('',(#1748,#1749,#1750,#1751));
#1830=CLOSED_SHELL('',(#1752,#1753,#1754,#1755,#1756,#1757));
#1831=CLOSED_SHELL('',(#1758,#1759,#1760,#1761,#1762,#1763,#1764,#1765,
#1766,#1767,#1768,#1769,#1770,#1771,#1772,#1773,#1774,#1775,#1776,#1777,
#1778,#1779,#1780,#1781,#1782,#1783,#1784,#1785));
#1832=CLOSED_SHELL('',(#1786,#1787,#1788,#1789,#1790,#1791,#1792,#1793,
#1794,#1795,#1796,#1797,#1798,#1799,#1800,#1801,#1802,#1803,#1804));
#1833=CLOSED_SHELL('',(#1805,#1806,#1807,#1808,#1809,#1810,#1811,#1812,
#1813,#1814,#1815,#1816,#1817,#1818,#1819,#1820,#1821,#1822,#1823,#1824,
#1825));
#1834=DERIVED_UNIT_ELEMENT(#1850,1.);
#1835=DERIVED_UNIT_ELEMENT(#14546,-3.);
#1836=DERIVED_UNIT_ELEMENT(#1850,1.);
#1837=DERIVED_UNIT_ELEMENT(#14546,-3.);
#1838=DERIVED_UNIT_ELEMENT(#1850,1.);
#1839=DERIVED_UNIT_ELEMENT(#14546,-3.);
#1840=DERIVED_UNIT_ELEMENT(#1850,1.);
#1841=DERIVED_UNIT_ELEMENT(#14546,-3.);
#1842=DERIVED_UNIT_ELEMENT(#1850,1.);
#1843=DERIVED_UNIT_ELEMENT(#14546,-3.);
#1844=DERIVED_UNIT_ELEMENT(#1850,1.);
#1845=DERIVED_UNIT_ELEMENT(#14546,-3.);
#1846=DERIVED_UNIT_ELEMENT(#1850,1.);
#1847=DERIVED_UNIT_ELEMENT(#14546,-3.);
#1848=DERIVED_UNIT_ELEMENT(#1850,1.);
#1849=DERIVED_UNIT_ELEMENT(#14546,-3.);
#1850=(
MASS_UNIT()
NAMED_UNIT(*)
SI_UNIT(.KILO.,.GRAM.)
);
#1851=DERIVED_UNIT((#1834,#1835));
#1852=DERIVED_UNIT((#1836,#1837));
#1853=DERIVED_UNIT((#1838,#1839));
#1854=DERIVED_UNIT((#1840,#1841));
#1855=DERIVED_UNIT((#1842,#1843));
#1856=DERIVED_UNIT((#1844,#1845));
#1857=DERIVED_UNIT((#1846,#1847));
#1858=DERIVED_UNIT((#1848,#1849));
#1859=MEASURE_REPRESENTATION_ITEM('density measure',
POSITIVE_RATIO_MEASURE(7850.),#1851);
#1860=MEASURE_REPRESENTATION_ITEM('density measure',
POSITIVE_RATIO_MEASURE(7850.),#1852);
#1861=MEASURE_REPRESENTATION_ITEM('density measure',
POSITIVE_RATIO_MEASURE(7850.),#1853);
#1862=MEASURE_REPRESENTATION_ITEM('density measure',
POSITIVE_RATIO_MEASURE(7850.),#1854);
#1863=MEASURE_REPRESENTATION_ITEM('density measure',
POSITIVE_RATIO_MEASURE(7850.),#1855);
#1864=MEASURE_REPRESENTATION_ITEM('density measure',
POSITIVE_RATIO_MEASURE(7850.),#1856);
#1865=MEASURE_REPRESENTATION_ITEM('density measure',
POSITIVE_RATIO_MEASURE(7850.),#1857);
#1866=MEASURE_REPRESENTATION_ITEM('density measure',
POSITIVE_RATIO_MEASURE(7850.),#1858);
#1867=PROPERTY_DEFINITION_REPRESENTATION(#1907,#1883);
#1868=PROPERTY_DEFINITION_REPRESENTATION(#1908,#1884);
#1869=PROPERTY_DEFINITION_REPRESENTATION(#1909,#1885);
#1870=PROPERTY_DEFINITION_REPRESENTATION(#1910,#1886);
#1871=PROPERTY_DEFINITION_REPRESENTATION(#1911,#1887);
#1872=PROPERTY_DEFINITION_REPRESENTATION(#1912,#1888);
#1873=PROPERTY_DEFINITION_REPRESENTATION(#1913,#1889);
#1874=PROPERTY_DEFINITION_REPRESENTATION(#1914,#1890);
#1875=PROPERTY_DEFINITION_REPRESENTATION(#1915,#1891);
#1876=PROPERTY_DEFINITION_REPRESENTATION(#1916,#1892);
#1877=PROPERTY_DEFINITION_REPRESENTATION(#1917,#1893);
#1878=PROPERTY_DEFINITION_REPRESENTATION(#1918,#1894);
#1879=PROPERTY_DEFINITION_REPRESENTATION(#1919,#1895);
#1880=PROPERTY_DEFINITION_REPRESENTATION(#1920,#1896);
#1881=PROPERTY_DEFINITION_REPRESENTATION(#1921,#1897);
#1882=PROPERTY_DEFINITION_REPRESENTATION(#1922,#1898);
#1883=REPRESENTATION('material name',(#1899),#14536);
#1884=REPRESENTATION('density',(#1859),#14536);
#1885=REPRESENTATION('material name',(#1900),#14537);
#1886=REPRESENTATION('density',(#1860),#14537);
#1887=REPRESENTATION('material name',(#1901),#14538);
#1888=REPRESENTATION('density',(#1861),#14538);
#1889=REPRESENTATION('material name',(#1902),#14539);
#1890=REPRESENTATION('density',(#1862),#14539);
#1891=REPRESENTATION('material name',(#1903),#14540);
#1892=REPRESENTATION('density',(#1863),#14540);
#1893=REPRESENTATION('material name',(#1904),#14541);
#1894=REPRESENTATION('density',(#1864),#14541);
#1895=REPRESENTATION('material name',(#1905),#14542);
#1896=REPRESENTATION('density',(#1865),#14542);
#1897=REPRESENTATION('material name',(#1906),#14543);
#1898=REPRESENTATION('density',(#1866),#14543);
#1899=DESCRIPTIVE_REPRESENTATION_ITEM('Steel','Steel');
#1900=DESCRIPTIVE_REPRESENTATION_ITEM('Steel','Steel');
#1901=DESCRIPTIVE_REPRESENTATION_ITEM('Steel','Steel');
#1902=DESCRIPTIVE_REPRESENTATION_ITEM('Steel','Steel');
#1903=DESCRIPTIVE_REPRESENTATION_ITEM('Steel','Steel');
#1904=DESCRIPTIVE_REPRESENTATION_ITEM('Steel','Steel');
#1905=DESCRIPTIVE_REPRESENTATION_ITEM('Steel','Steel');
#1906=DESCRIPTIVE_REPRESENTATION_ITEM('Steel','Steel');
#1907=PROPERTY_DEFINITION('material property','material name',#14586);
#1908=PROPERTY_DEFINITION('material property','density of part',#14586);
#1909=PROPERTY_DEFINITION('material property','material name',#14587);
#1910=PROPERTY_DEFINITION('material property','density of part',#14587);
#1911=PROPERTY_DEFINITION('material property','material name',#14588);
#1912=PROPERTY_DEFINITION('material property','density of part',#14588);
#1913=PROPERTY_DEFINITION('material property','material name',#14589);
#1914=PROPERTY_DEFINITION('material property','density of part',#14589);
#1915=PROPERTY_DEFINITION('material property','material name',#14590);
#1916=PROPERTY_DEFINITION('material property','density of part',#14590);
#1917=PROPERTY_DEFINITION('material property','material name',#14591);
#1918=PROPERTY_DEFINITION('material property','density of part',#14591);
#1919=PROPERTY_DEFINITION('material property','material name',#14592);
#1920=PROPERTY_DEFINITION('material property','density of part',#14592);
#1921=PROPERTY_DEFINITION('material property','material name',#14593);
#1922=PROPERTY_DEFINITION('material property','density of part',#14593);
#1923=AXIS2_PLACEMENT_3D('',#2594,#2128,#2129);
#1924=AXIS2_PLACEMENT_3D('',#2595,#2130,#2131);
#1925=AXIS2_PLACEMENT_3D('',#2596,#2132,#2133);
#1926=AXIS2_PLACEMENT_3D('',#2598,#2134,#2135);
#1927=AXIS2_PLACEMENT_3D('',#2600,#2136,#2137);
#1928=AXIS2_PLACEMENT_3D('',#2601,#2138,#2139);
#1929=AXIS2_PLACEMENT_3D('',#2603,#2140,#2141);
#1930=AXIS2_PLACEMENT_3D('',#2605,#2142,#2143);
#1931=AXIS2_PLACEMENT_3D('',#2606,#2144,#2145);
#1932=AXIS2_PLACEMENT_3D('',#2608,#2147,#2148);
#1933=AXIS2_PLACEMENT_3D('',#2610,#2150,#2151);
#1934=AXIS2_PLACEMENT_3D('',#2611,#2152,#2153);
#1935=AXIS2_PLACEMENT_3D('',#2613,#2154,#2155);
#1936=AXIS2_PLACEMENT_3D('',#2614,#2156,#2157);
#1937=AXIS2_PLACEMENT_3D('',#2616,#2158,#2159);
#1938=AXIS2_PLACEMENT_3D('',#2619,#2161,#2162);
#1939=AXIS2_PLACEMENT_3D('',#2620,#2163,#2164);
#1940=AXIS2_PLACEMENT_3D('',#2622,#2165,#2166);
#1941=AXIS2_PLACEMENT_3D('',#2623,#2167,#2168);
#1942=AXIS2_PLACEMENT_3D('',#2626,#2170,#2171);
#1943=AXIS2_PLACEMENT_3D('',#2627,#2172,#2173);
#1944=AXIS2_PLACEMENT_3D('',#2629,#2174,#2175);
#1945=AXIS2_PLACEMENT_3D('',#2630,#2176,#2177);
#1946=AXIS2_PLACEMENT_3D('',#2633,#2179,#2180);
#1947=AXIS2_PLACEMENT_3D('',#2634,#2181,#2182);
#1948=AXIS2_PLACEMENT_3D('',#2636,#2183,#2184);
#1949=AXIS2_PLACEMENT_3D('',#2637,#2185,#2186);
#1950=AXIS2_PLACEMENT_3D('',#2640,#2188,#2189);
#1951=AXIS2_PLACEMENT_3D('',#2641,#2190,#2191);
#1952=AXIS2_PLACEMENT_3D('',#2643,#2192,#2193);
#1953=AXIS2_PLACEMENT_3D('',#2644,#2194,#2195);
#1954=AXIS2_PLACEMENT_3D('',#2645,#2196,#2197);
#1955=AXIS2_PLACEMENT_3D('',#2647,#2198,#2199);
#1956=AXIS2_PLACEMENT_3D('',#2648,#2200,#2201);
#1957=AXIS2_PLACEMENT_3D('',#2651,#2203,#2204);
#1958=AXIS2_PLACEMENT_3D('',#2652,#2205,#2206);
#1959=AXIS2_PLACEMENT_3D('',#2654,#2207,#2208);
#1960=AXIS2_PLACEMENT_3D('',#2655,#2209,#2210);
#1961=AXIS2_PLACEMENT_3D('',#2658,#2212,#2213);
#1962=AXIS2_PLACEMENT_3D('',#2659,#2214,#2215);
#1963=AXIS2_PLACEMENT_3D('',#2660,#2216,#2217);
#1964=AXIS2_PLACEMENT_3D('',#2662,#2218,#2219);
#1965=AXIS2_PLACEMENT_3D('',#2663,#2220,#2221);
#1966=AXIS2_PLACEMENT_3D('',#2665,#2223,#2224);
#1967=AXIS2_PLACEMENT_3D('',#2666,#2225,#2226);
#1968=AXIS2_PLACEMENT_3D('',#2668,#2227,#2228);
#1969=AXIS2_PLACEMENT_3D('',#2671,#2230,#2231);
#1970=AXIS2_PLACEMENT_3D('',#2672,#2232,#2233);
#1971=AXIS2_PLACEMENT_3D('',#2674,#2234,#2235);
#1972=AXIS2_PLACEMENT_3D('',#2675,#2236,#2237);
#1973=AXIS2_PLACEMENT_3D('',#2677,#2238,#2239);
#1974=AXIS2_PLACEMENT_3D('',#2679,#2241,#2242);
#1975=AXIS2_PLACEMENT_3D('',#2681,#2243,#2244);
#1976=AXIS2_PLACEMENT_3D('',#2682,#2245,#2246);
#1977=AXIS2_PLACEMENT_3D('',#2684,#2247,#2248);
#1978=AXIS2_PLACEMENT_3D('',#2686,#2250,#2251);
#1979=AXIS2_PLACEMENT_3D('',#2688,#2252,#2253);
#1980=AXIS2_PLACEMENT_3D('',#2689,#2254,#2255);
#1981=AXIS2_PLACEMENT_3D('',#2691,#2256,#2257);
#1982=AXIS2_PLACEMENT_3D('',#2692,#2258,#2259);
#1983=AXIS2_PLACEMENT_3D('',#2693,#2260,#2261);
#1984=AXIS2_PLACEMENT_3D('',#2695,#2262,#2263);
#1985=AXIS2_PLACEMENT_3D('',#2697,#2264,#2265);
#1986=AXIS2_PLACEMENT_3D('',#2698,#2266,#2267);
#1987=AXIS2_PLACEMENT_3D('',#2700,#2268,#2269);
#1988=AXIS2_PLACEMENT_3D('',#2702,#2271,#2272);
#1989=AXIS2_PLACEMENT_3D('',#2704,#2273,#2274);
#1990=AXIS2_PLACEMENT_3D('',#2705,#2275,#2276);
#1991=AXIS2_PLACEMENT_3D('',#2707,#2278,#2279);
#1992=AXIS2_PLACEMENT_3D('',#2708,#2280,#2281);
#1993=AXIS2_PLACEMENT_3D('',#2710,#2282,#2283);
#1994=AXIS2_PLACEMENT_3D('',#2713,#2285,#2286);
#1995=AXIS2_PLACEMENT_3D('',#2714,#2287,#2288);
#1996=AXIS2_PLACEMENT_3D('',#2716,#2289,#2290);
#1997=AXIS2_PLACEMENT_3D('',#2717,#2291,#2292);
#1998=AXIS2_PLACEMENT_3D('',#2719,#2293,#2294);
#1999=AXIS2_PLACEMENT_3D('',#2721,#2296,#2297);
#2000=AXIS2_PLACEMENT_3D('',#2723,#2298,#2299);
#2001=AXIS2_PLACEMENT_3D('',#2724,#2300,#2301);
#2002=AXIS2_PLACEMENT_3D('',#2726,#2302,#2303);
#2003=AXIS2_PLACEMENT_3D('',#2728,#2305,#2306);
#2004=AXIS2_PLACEMENT_3D('',#2729,#2307,#2308);
#2005=AXIS2_PLACEMENT_3D('',#2730,#2309,#2310);
#2006=AXIS2_PLACEMENT_3D('',#2866,#2312,#2313);
#2007=AXIS2_PLACEMENT_3D('',#2964,#2314,#2315);
#2008=AXIS2_PLACEMENT_3D('',#3173,#2317,#2318);
#2009=AXIS2_PLACEMENT_3D('',#3541,#2320,#2321);
#2010=AXIS2_PLACEMENT_3D('',#3926,#2323,#2324);
#2011=AXIS2_PLACEMENT_3D('',#4291,#2326,#2327);
#2012=AXIS2_PLACEMENT_3D('',#4658,#2329,#2330);
#2013=AXIS2_PLACEMENT_3D('',#5033,#2332,#2333);
#2014=AXIS2_PLACEMENT_3D('',#5400,#2335,#2336);
#2015=AXIS2_PLACEMENT_3D('',#5769,#2338,#2339);
#2016=AXIS2_PLACEMENT_3D('',#6146,#2341,#2342);
#2017=AXIS2_PLACEMENT_3D('',#6511,#2344,#2345);
#2018=AXIS2_PLACEMENT_3D('',#6521,#2346,#2347);
#2019=AXIS2_PLACEMENT_3D('',#6991,#2348,#2349);
#2020=AXIS2_PLACEMENT_3D('',#7310,#2350,#2351);
#2021=AXIS2_PLACEMENT_3D('',#7467,#2352,#2353);
#2022=AXIS2_PLACEMENT_3D('',#8559,#2354,#2355);
#2023=AXIS2_PLACEMENT_3D('',#8561,#2356,#2357);
#2024=AXIS2_PLACEMENT_3D('',#8562,#2358,#2359);
#2025=AXIS2_PLACEMENT_3D('',#8563,#2360,#2361);
#2026=AXIS2_PLACEMENT_3D('',#8565,#2362,#2363);
#2027=AXIS2_PLACEMENT_3D('',#8566,#2364,#2365);
#2028=AXIS2_PLACEMENT_3D('',#8568,#2366,#2367);
#2029=AXIS2_PLACEMENT_3D('',#8570,#2369,#2370);
#2030=AXIS2_PLACEMENT_3D('',#8573,#2372,#2373);
#2031=AXIS2_PLACEMENT_3D('',#8574,#2374,#2375);
#2032=AXIS2_PLACEMENT_3D('',#8576,#2376,#2377);
#2033=AXIS2_PLACEMENT_3D('',#8578,#2379,#2380);
#2034=AXIS2_PLACEMENT_3D('',#8580,#2381,#2382);
#2035=AXIS2_PLACEMENT_3D('',#8581,#2383,#2384);
#2036=AXIS2_PLACEMENT_3D('',#8583,#2385,#2386);
#2037=AXIS2_PLACEMENT_3D('',#8585,#2388,#2389);
#2038=AXIS2_PLACEMENT_3D('',#8587,#2390,#2391);
#2039=AXIS2_PLACEMENT_3D('',#8588,#2392,#2393);
#2040=AXIS2_PLACEMENT_3D('',#8589,#2394,#2395);
#2041=AXIS2_PLACEMENT_3D('',#8591,#2396,#2397);
#2042=AXIS2_PLACEMENT_3D('',#8592,#2398,#2399);
#2043=AXIS2_PLACEMENT_3D('',#8594,#2400,#2401);
#2044=AXIS2_PLACEMENT_3D('',#8596,#2403,#2404);
#2045=AXIS2_PLACEMENT_3D('',#8598,#2405,#2406);
#2046=AXIS2_PLACEMENT_3D('',#8599,#2407,#2408);
#2047=AXIS2_PLACEMENT_3D('',#8601,#2410,#2411);
#2048=AXIS2_PLACEMENT_3D('',#8602,#2412,#2413);
#2049=AXIS2_PLACEMENT_3D('',#8604,#2414,#2415);
#2050=AXIS2_PLACEMENT_3D('',#8606,#2416,#2417);
#2051=AXIS2_PLACEMENT_3D('',#8607,#2418,#2419);
#2052=AXIS2_PLACEMENT_3D('',#8610,#2421,#2422);
#2053=AXIS2_PLACEMENT_3D('',#8611,#2423,#2424);
#2054=AXIS2_PLACEMENT_3D('',#8613,#2425,#2426);
#2055=AXIS2_PLACEMENT_3D('',#8614,#2427,#2428);
#2056=AXIS2_PLACEMENT_3D('',#8616,#2429,#2430);
#2057=AXIS2_PLACEMENT_3D('',#8618,#2432,#2433);
#2058=AXIS2_PLACEMENT_3D('',#8620,#2434,#2435);
#2059=AXIS2_PLACEMENT_3D('',#8621,#2436,#2437);
#2060=AXIS2_PLACEMENT_3D('',#8623,#2438,#2439);
#2061=AXIS2_PLACEMENT_3D('',#8625,#2441,#2442);
#2062=AXIS2_PLACEMENT_3D('',#8628,#2444,#2445);
#2063=AXIS2_PLACEMENT_3D('',#8629,#2446,#2447);
#2064=AXIS2_PLACEMENT_3D('',#8631,#2448,#2449);
#2065=AXIS2_PLACEMENT_3D('',#8632,#2450,#2451);
#2066=AXIS2_PLACEMENT_3D('',#8635,#2453,#2454);
#2067=AXIS2_PLACEMENT_3D('',#8636,#2455,#2456);
#2068=AXIS2_PLACEMENT_3D('',#8638,#2457,#2458);
#2069=AXIS2_PLACEMENT_3D('',#8639,#2459,#2460);
#2070=AXIS2_PLACEMENT_3D('',#8641,#2461,#2462);
#2071=AXIS2_PLACEMENT_3D('',#8643,#2464,#2465);
#2072=AXIS2_PLACEMENT_3D('',#8645,#2466,#2467);
#2073=AXIS2_PLACEMENT_3D('',#8646,#2468,#2469);
#2074=AXIS2_PLACEMENT_3D('',#8648,#2470,#2471);
#2075=AXIS2_PLACEMENT_3D('',#8650,#2473,#2474);
#2076=AXIS2_PLACEMENT_3D('',#8652,#2475,#2476);
#2077=AXIS2_PLACEMENT_3D('',#8653,#2477,#2478);
#2078=AXIS2_PLACEMENT_3D('',#8655,#2479,#2480);
#2079=AXIS2_PLACEMENT_3D('',#8657,#2482,#2483);
#2080=AXIS2_PLACEMENT_3D('',#8659,#2484,#2485);
#2081=AXIS2_PLACEMENT_3D('',#8660,#2486,#2487);
#2082=AXIS2_PLACEMENT_3D('',#8662,#2488,#2489);
#2083=AXIS2_PLACEMENT_3D('',#8664,#2491,#2492);
#2084=AXIS2_PLACEMENT_3D('',#8666,#2493,#2494);
#2085=AXIS2_PLACEMENT_3D('',#8668,#2496,#2497);
#2086=AXIS2_PLACEMENT_3D('',#8670,#2499,#2500);
#2087=AXIS2_PLACEMENT_3D('',#8671,#2501,#2502);
#2088=AXIS2_PLACEMENT_3D('',#8685,#2504,#2505);
#2089=AXIS2_PLACEMENT_3D('',#8780,#2506,#2507);
#2090=AXIS2_PLACEMENT_3D('',#9126,#2509,#2510);
#2091=AXIS2_PLACEMENT_3D('',#9475,#2512,#2513);
#2092=AXIS2_PLACEMENT_3D('',#9799,#2515,#2516);
#2093=AXIS2_PLACEMENT_3D('',#10143,#2518,#2519);
#2094=AXIS2_PLACEMENT_3D('',#10471,#2521,#2522);
#2095=AXIS2_PLACEMENT_3D('',#10807,#2524,#2525);
#2096=AXIS2_PLACEMENT_3D('',#10875,#2526,#2527);
#2097=AXIS2_PLACEMENT_3D('',#12285,#2528,#2529);
#2098=AXIS2_PLACEMENT_3D('',#13457,#2530,#2531);
#2099=AXIS2_PLACEMENT_3D('',#13602,#2532,#2533);
#2100=AXIS2_PLACEMENT_3D('',#14097,#2534,#2535);
#2101=AXIS2_PLACEMENT_3D('',#14099,#2536,#2537);
#2102=AXIS2_PLACEMENT_3D('',#14101,#2538,#2539);
#2103=AXIS2_PLACEMENT_3D('',#14489,#2540,#2541);
#2104=AXIS2_PLACEMENT_3D('',#14491,#2542,#2543);
#2105=AXIS2_PLACEMENT_3D('',#14492,#2544,#2545);
#2106=AXIS2_PLACEMENT_3D('',#14493,#2546,#2547);
#2107=AXIS2_PLACEMENT_3D('',#14495,#2548,#2549);
#2108=AXIS2_PLACEMENT_3D('',#14496,#2550,#2551);
#2109=AXIS2_PLACEMENT_3D('',#14498,#2552,#2553);
#2110=AXIS2_PLACEMENT_3D('',#14500,#2555,#2556);
#2111=AXIS2_PLACEMENT_3D('',#14503,#2558,#2559);
#2112=AXIS2_PLACEMENT_3D('',#14504,#2560,#2561);
#2113=AXIS2_PLACEMENT_3D('',#14506,#2562,#2563);
#2114=AXIS2_PLACEMENT_3D('',#14507,#2564,#2565);
#2115=AXIS2_PLACEMENT_3D('',#14509,#2566,#2567);
#2116=AXIS2_PLACEMENT_3D('',#14511,#2569,#2570);
#2117=AXIS2_PLACEMENT_3D('',#14512,#2571,#2572);
#2118=AXIS2_PLACEMENT_3D('',#14514,#2573,#2574);
#2119=AXIS2_PLACEMENT_3D('',#14515,#2575,#2576);
#2120=AXIS2_PLACEMENT_3D('',#14517,#2578,#2579);
#2121=AXIS2_PLACEMENT_3D('',#14518,#2580,#2581);
#2122=AXIS2_PLACEMENT_3D('',#14519,#2582,#2583);
#2123=AXIS2_PLACEMENT_3D('',#14520,#2584,#2585);
#2124=AXIS2_PLACEMENT_3D('',#14521,#2586,#2587);
#2125=AXIS2_PLACEMENT_3D('',#14522,#2588,#2589);
#2126=AXIS2_PLACEMENT_3D('',#14523,#2590,#2591);
#2127=AXIS2_PLACEMENT_3D('',#14524,#2592,#2593);
#2128=DIRECTION('axis',(0.,0.,1.));
#2129=DIRECTION('refdir',(1.,0.,0.));
#2130=DIRECTION('axis',(0.,0.,1.));
#2131=DIRECTION('refdir',(1.,0.,0.));
#2132=DIRECTION('center_axis',(0.,0.,1.));
#2133=DIRECTION('ref_axis',(1.,0.,0.));
#2134=DIRECTION('center_axis',(0.,0.,1.));
#2135=DIRECTION('ref_axis',(1.,0.,0.));
#2136=DIRECTION('center_axis',(0.,0.,1.));
#2137=DIRECTION('ref_axis',(1.,0.,0.));
#2138=DIRECTION('center_axis',(0.,0.,-1.));
#2139=DIRECTION('ref_axis',(-1.,0.,0.));
#2140=DIRECTION('center_axis',(0.,0.,1.));
#2141=DIRECTION('ref_axis',(1.,0.,0.));
#2142=DIRECTION('center_axis',(0.,0.,1.));
#2143=DIRECTION('ref_axis',(1.,0.,0.));
#2144=DIRECTION('center_axis',(0.,0.,1.));
#2145=DIRECTION('ref_axis',(1.,0.,0.));
#2146=DIRECTION('',(0.,0.,1.));
#2147=DIRECTION('center_axis',(0.,0.,1.));
#2148=DIRECTION('ref_axis',(1.,0.,0.));
#2149=DIRECTION('',(0.,0.,-1.));
#2150=DIRECTION('axis',(0.,0.,1.));
#2151=DIRECTION('refdir',(1.,0.,0.));
#2152=DIRECTION('center_axis',(0.,0.,1.));
#2153=DIRECTION('ref_axis',(1.,0.,0.));
#2154=DIRECTION('center_axis',(0.,0.,1.));
#2155=DIRECTION('ref_axis',(1.,0.,0.));
#2156=DIRECTION('center_axis',(0.,0.,1.));
#2157=DIRECTION('ref_axis',(1.,0.,0.));
#2158=DIRECTION('center_axis',(0.,0.,1.));
#2159=DIRECTION('ref_axis',(1.,0.,0.));
#2160=DIRECTION('',(0.,0.,-1.));
#2161=DIRECTION('center_axis',(0.,0.,1.));
#2162=DIRECTION('ref_axis',(1.,0.,0.));
#2163=DIRECTION('center_axis',(0.,0.,-1.));
#2164=DIRECTION('ref_axis',(-1.,0.,0.));
#2165=DIRECTION('center_axis',(0.,0.,1.));
#2166=DIRECTION('ref_axis',(1.,0.,0.));
#2167=DIRECTION('center_axis',(0.,0.,1.));
#2168=DIRECTION('ref_axis',(1.,0.,0.));
#2169=DIRECTION('',(0.,0.,1.));
#2170=DIRECTION('center_axis',(0.,0.,1.));
#2171=DIRECTION('ref_axis',(1.,0.,0.));
#2172=DIRECTION('center_axis',(0.,0.,-1.));
#2173=DIRECTION('ref_axis',(-1.,0.,0.));
#2174=DIRECTION('center_axis',(0.,0.,1.));
#2175=DIRECTION('ref_axis',(1.,0.,0.));
#2176=DIRECTION('center_axis',(0.,0.,1.));
#2177=DIRECTION('ref_axis',(1.,0.,0.));
#2178=DIRECTION('',(0.,0.,-1.));
#2179=DIRECTION('center_axis',(0.,0.,1.));
#2180=DIRECTION('ref_axis',(1.,0.,0.));
#2181=DIRECTION('center_axis',(0.,0.,1.));
#2182=DIRECTION('ref_axis',(1.,0.,0.));
#2183=DIRECTION('center_axis',(0.,0.,1.));
#2184=DIRECTION('ref_axis',(1.,0.,0.));
#2185=DIRECTION('center_axis',(0.,0.,1.));
#2186=DIRECTION('ref_axis',(1.,0.,0.));
#2187=DIRECTION('',(0.,0.,-1.));
#2188=DIRECTION('center_axis',(0.,0.,1.));
#2189=DIRECTION('ref_axis',(1.,0.,0.));
#2190=DIRECTION('center_axis',(0.,0.,1.));
#2191=DIRECTION('ref_axis',(1.,0.,0.));
#2192=DIRECTION('center_axis',(1.22464679914735E-16,-1.,0.));
#2193=DIRECTION('ref_axis',(-1.,-1.22464679914735E-16,0.));
#2194=DIRECTION('center_axis',(0.,0.,1.));
#2195=DIRECTION('ref_axis',(1.,0.,0.));
#2196=DIRECTION('center_axis',(0.,0.,-1.));
#2197=DIRECTION('ref_axis',(-1.,0.,0.));
#2198=DIRECTION('center_axis',(0.,0.,1.));
#2199=DIRECTION('ref_axis',(1.,0.,0.));
#2200=DIRECTION('center_axis',(0.,0.,1.));
#2201=DIRECTION('ref_axis',(1.,0.,0.));
#2202=DIRECTION('',(0.,0.,1.));
#2203=DIRECTION('center_axis',(0.,0.,1.));
#2204=DIRECTION('ref_axis',(1.,0.,0.));
#2205=DIRECTION('center_axis',(0.,0.,1.));
#2206=DIRECTION('ref_axis',(1.,0.,0.));
#2207=DIRECTION('center_axis',(0.,0.,1.));
#2208=DIRECTION('ref_axis',(1.,0.,0.));
#2209=DIRECTION('center_axis',(0.,0.,1.));
#2210=DIRECTION('ref_axis',(1.,0.,0.));
#2211=DIRECTION('',(0.,0.,1.));
#2212=DIRECTION('center_axis',(0.,0.,1.));
#2213=DIRECTION('ref_axis',(1.,0.,0.));
#2214=DIRECTION('center_axis',(0.,0.,-1.));
#2215=DIRECTION('ref_axis',(-1.,0.,0.));
#2216=DIRECTION('center_axis',(0.,0.,-1.));
#2217=DIRECTION('ref_axis',(-1.,0.,0.));
#2218=DIRECTION('center_axis',(0.,0.,-1.));
#2219=DIRECTION('ref_axis',(1.,0.,0.));
#2220=DIRECTION('center_axis',(0.,0.,1.));
#2221=DIRECTION('ref_axis',(1.,0.,0.));
#2222=DIRECTION('',(0.,0.,1.));
#2223=DIRECTION('axis',(0.,0.,1.));
#2224=DIRECTION('refdir',(1.,0.,0.));
#2225=DIRECTION('center_axis',(0.,0.,1.));
#2226=DIRECTION('ref_axis',(1.,0.,0.));
#2227=DIRECTION('center_axis',(0.,0.,1.));
#2228=DIRECTION('ref_axis',(1.,0.,0.));
#2229=DIRECTION('',(0.,0.,-1.));
#2230=DIRECTION('center_axis',(0.,0.,1.));
#2231=DIRECTION('ref_axis',(1.,0.,0.));
#2232=DIRECTION('center_axis',(0.,0.,-1.));
#2233=DIRECTION('ref_axis',(-1.,0.,0.));
#2234=DIRECTION('center_axis',(0.,0.,1.));
#2235=DIRECTION('ref_axis',(1.,0.,0.));
#2236=DIRECTION('center_axis',(0.,0.,1.));
#2237=DIRECTION('ref_axis',(1.,0.,0.));
#2238=DIRECTION('center_axis',(0.,0.,1.));
#2239=DIRECTION('ref_axis',(1.,0.,0.));
#2240=DIRECTION('',(0.,0.,-1.));
#2241=DIRECTION('center_axis',(0.,0.,1.));
#2242=DIRECTION('ref_axis',(1.,0.,0.));
#2243=DIRECTION('center_axis',(0.,0.,1.));
#2244=DIRECTION('ref_axis',(1.,0.,0.));
#2245=DIRECTION('center_axis',(0.,0.,1.));
#2246=DIRECTION('ref_axis',(1.,0.,0.));
#2247=DIRECTION('center_axis',(0.,0.,1.));
#2248=DIRECTION('ref_axis',(1.,0.,0.));
#2249=DIRECTION('',(0.,0.,-1.));
#2250=DIRECTION('center_axis',(1.22464679914735E-16,0.,1.));
#2251=DIRECTION('ref_axis',(1.,0.,0.));
#2252=DIRECTION('center_axis',(1.22464679914735E-16,-1.,-7.49879891330929E-33));
#2253=DIRECTION('ref_axis',(-1.,-1.22464679914735E-16,0.));
#2254=DIRECTION('center_axis',(1.22464679914735E-16,0.,1.));
#2255=DIRECTION('ref_axis',(1.,0.,0.));
#2256=DIRECTION('center_axis',(1.22464679914735E-16,-1.,-7.49879891330928E-33));
#2257=DIRECTION('ref_axis',(-1.,-1.22464679914735E-16,0.));
#2258=DIRECTION('axis',(0.,0.,1.));
#2259=DIRECTION('refdir',(1.,0.,0.));
#2260=DIRECTION('center_axis',(0.,0.,1.));
#2261=DIRECTION('ref_axis',(1.,0.,0.));
#2262=DIRECTION('center_axis',(0.,0.,1.));
#2263=DIRECTION('ref_axis',(1.,0.,0.));
#2264=DIRECTION('center_axis',(0.,0.,-1.));
#2265=DIRECTION('ref_axis',(1.,0.,0.));
#2266=DIRECTION('center_axis',(0.,0.,1.));
#2267=DIRECTION('ref_axis',(1.,0.,0.));
#2268=DIRECTION('center_axis',(0.,0.,1.));
#2269=DIRECTION('ref_axis',(1.,0.,0.));
#2270=DIRECTION('',(0.,0.,-1.));
#2271=DIRECTION('center_axis',(0.,0.,1.));
#2272=DIRECTION('ref_axis',(1.,0.,0.));
#2273=DIRECTION('center_axis',(0.,0.,1.));
#2274=DIRECTION('ref_axis',(1.,0.,0.));
#2275=DIRECTION('center_axis',(0.,0.,1.));
#2276=DIRECTION('ref_axis',(1.,0.,0.));
#2277=DIRECTION('',(0.,0.,1.));
#2278=DIRECTION('axis',(0.,0.,1.));
#2279=DIRECTION('refdir',(1.,0.,0.));
#2280=DIRECTION('center_axis',(0.,0.,1.));
#2281=DIRECTION('ref_axis',(1.,0.,0.));
#2282=DIRECTION('center_axis',(0.,0.,1.));
#2283=DIRECTION('ref_axis',(1.,0.,0.));
#2284=DIRECTION('',(0.,0.,1.));
#2285=DIRECTION('center_axis',(0.,0.,1.));
#2286=DIRECTION('ref_axis',(1.,0.,0.));
#2287=DIRECTION('center_axis',(0.,0.,-1.));
#2288=DIRECTION('ref_axis',(-1.,0.,0.));
#2289=DIRECTION('center_axis',(0.,0.,1.));
#2290=DIRECTION('ref_axis',(1.,0.,0.));
#2291=DIRECTION('center_axis',(0.,0.,1.));
#2292=DIRECTION('ref_axis',(1.,0.,0.));
#2293=DIRECTION('center_axis',(0.,0.,1.));
#2294=DIRECTION('ref_axis',(1.,0.,0.));
#2295=DIRECTION('',(0.,0.,-1.));
#2296=DIRECTION('center_axis',(0.,0.,1.));
#2297=DIRECTION('ref_axis',(1.,0.,0.));
#2298=DIRECTION('center_axis',(0.,0.,1.));
#2299=DIRECTION('ref_axis',(1.,0.,0.));
#2300=DIRECTION('center_axis',(0.,0.,1.));
#2301=DIRECTION('ref_axis',(1.,0.,0.));
#2302=DIRECTION('center_axis',(0.,0.,1.));
#2303=DIRECTION('ref_axis',(1.,0.,0.));
#2304=DIRECTION('',(0.,0.,1.));
#2305=DIRECTION('center_axis',(0.,0.,1.));
#2306=DIRECTION('ref_axis',(1.,0.,0.));
#2307=DIRECTION('axis',(0.,0.,1.));
#2308=DIRECTION('refdir',(1.,0.,0.));
#2309=DIRECTION('center_axis',(0.,0.,1.));
#2310=DIRECTION('ref_axis',(0.839955785831598,-0.542654842278241,0.));
#2311=DIRECTION('',(0.,0.,-1.));
#2312=DIRECTION('center_axis',(0.,0.,-1.));
#2313=DIRECTION('ref_axis',(1.,5.80632514073727E-14,0.));
#2314=DIRECTION('center_axis',(0.,0.,1.));
#2315=DIRECTION('ref_axis',(0.839955785831598,-0.542654842278241,0.));
#2316=DIRECTION('',(0.,0.,-1.));
#2317=DIRECTION('center_axis',(0.,0.,1.));
#2318=DIRECTION('ref_axis',(0.839955785831598,-0.542654842278241,0.));
#2319=DIRECTION('',(0.,0.,-1.));
#2320=DIRECTION('center_axis',(0.,0.,1.));
#2321=DIRECTION('ref_axis',(0.839955785831598,-0.542654842278241,0.));
#2322=DIRECTION('',(0.,0.,-1.));
#2323=DIRECTION('center_axis',(0.,0.,1.));
#2324=DIRECTION('ref_axis',(0.839955785831598,-0.542654842278241,0.));
#2325=DIRECTION('',(0.,0.,-1.));
#2326=DIRECTION('center_axis',(0.,0.,1.));
#2327=DIRECTION('ref_axis',(0.839955785831598,-0.542654842278241,0.));
#2328=DIRECTION('',(0.,0.,-1.));
#2329=DIRECTION('center_axis',(0.,0.,1.));
#2330=DIRECTION('ref_axis',(0.839955785831598,-0.542654842278241,0.));
#2331=DIRECTION('',(0.,0.,-1.));
#2332=DIRECTION('center_axis',(0.,0.,1.));
#2333=DIRECTION('ref_axis',(0.839955785831598,-0.542654842278241,0.));
#2334=DIRECTION('',(0.,0.,-1.));
#2335=DIRECTION('center_axis',(0.,0.,1.));
#2336=DIRECTION('ref_axis',(0.839955785831598,-0.542654842278241,0.));
#2337=DIRECTION('',(0.,0.,-1.));
#2338=DIRECTION('center_axis',(0.,0.,1.));
#2339=DIRECTION('ref_axis',(0.839955785831598,-0.542654842278241,0.));
#2340=DIRECTION('',(0.,0.,-1.));
#2341=DIRECTION('center_axis',(0.,0.,1.));
#2342=DIRECTION('ref_axis',(0.839955785831598,-0.542654842278241,0.));
#2343=DIRECTION('',(0.,0.,-1.));
#2344=DIRECTION('center_axis',(0.,0.,1.));
#2345=DIRECTION('ref_axis',(1.,0.,0.));
#2346=DIRECTION('center_axis',(0.,0.,1.));
#2347=DIRECTION('ref_axis',(1.,0.,0.));
#2348=DIRECTION('center_axis',(0.,0.,1.));
#2349=DIRECTION('ref_axis',(1.,0.,0.));
#2350=DIRECTION('center_axis',(0.,0.,1.));
#2351=DIRECTION('ref_axis',(0.839955785831598,-0.542654842278241,0.));
#2352=DIRECTION('center_axis',(0.,0.,1.));
#2353=DIRECTION('ref_axis',(1.,5.80632514073727E-14,0.));
#2354=DIRECTION('center_axis',(0.,0.,1.));
#2355=DIRECTION('ref_axis',(1.,0.,0.));
#2356=DIRECTION('center_axis',(0.,0.,1.));
#2357=DIRECTION('ref_axis',(1.,0.,0.));
#2358=DIRECTION('center_axis',(0.,0.,-1.));
#2359=DIRECTION('ref_axis',(-1.,0.,0.));
#2360=DIRECTION('center_axis',(0.,0.,-1.));
#2361=DIRECTION('ref_axis',(-1.,0.,0.));
#2362=DIRECTION('center_axis',(0.,0.,1.));
#2363=DIRECTION('ref_axis',(1.,0.,0.));
#2364=DIRECTION('center_axis',(0.,0.,1.));
#2365=DIRECTION('ref_axis',(1.,0.,0.));
#2366=DIRECTION('center_axis',(0.,0.,1.));
#2367=DIRECTION('ref_axis',(1.,0.,0.));
#2368=DIRECTION('',(0.,0.,-1.));
#2369=DIRECTION('center_axis',(0.,0.,-1.));
#2370=DIRECTION('ref_axis',(1.,0.,0.));
#2371=DIRECTION('',(0.890347471651363,-1.09036118128678E-16,0.455281648788994));
#2372=DIRECTION('center_axis',(0.,0.,1.));
#2373=DIRECTION('ref_axis',(1.,0.,0.));
#2374=DIRECTION('center_axis',(0.,0.,1.));
#2375=DIRECTION('ref_axis',(1.,0.,0.));
#2376=DIRECTION('center_axis',(0.,0.,1.));
#2377=DIRECTION('ref_axis',(1.,0.,0.));
#2378=DIRECTION('',(0.,0.,-1.));
#2379=DIRECTION('center_axis',(0.,0.,-1.));
#2380=DIRECTION('ref_axis',(-1.,0.,0.));
#2381=DIRECTION('center_axis',(0.,0.,1.));
#2382=DIRECTION('ref_axis',(1.,0.,0.));
#2383=DIRECTION('center_axis',(0.,0.,1.));
#2384=DIRECTION('ref_axis',(1.,0.,0.));
#2385=DIRECTION('center_axis',(0.,0.,1.));
#2386=DIRECTION('ref_axis',(1.,0.,0.));
#2387=DIRECTION('',(0.,0.,-1.));
#2388=DIRECTION('center_axis',(0.,0.,1.));
#2389=DIRECTION('ref_axis',(1.,0.,0.));
#2390=DIRECTION('center_axis',(0.,0.,1.));
#2391=DIRECTION('ref_axis',(1.,0.,0.));
#2392=DIRECTION('center_axis',(1.22464679914735E-16,-1.,0.));
#2393=DIRECTION('ref_axis',(-1.,-1.22464679914735E-16,0.));
#2394=DIRECTION('center_axis',(0.,0.,1.));
#2395=DIRECTION('ref_axis',(1.,0.,0.));
#2396=DIRECTION('center_axis',(0.,0.,1.));
#2397=DIRECTION('ref_axis',(1.,0.,0.));
#2398=DIRECTION('center_axis',(0.,0.,1.));
#2399=DIRECTION('ref_axis',(1.,0.,0.));
#2400=DIRECTION('center_axis',(0.,0.,1.));
#2401=DIRECTION('ref_axis',(1.,0.,0.));
#2402=DIRECTION('',(0.,0.,1.));
#2403=DIRECTION('center_axis',(0.,0.,-1.));
#2404=DIRECTION('ref_axis',(-1.,0.,0.));
#2405=DIRECTION('center_axis',(0.,0.,1.));
#2406=DIRECTION('ref_axis',(1.,0.,0.));
#2407=DIRECTION('center_axis',(0.,0.,1.));
#2408=DIRECTION('ref_axis',(1.,0.,0.));
#2409=DIRECTION('',(0.,0.,1.));
#2410=DIRECTION('axis',(0.,0.,1.));
#2411=DIRECTION('refdir',(1.,0.,0.));
#2412=DIRECTION('center_axis',(0.,0.,-1.));
#2413=DIRECTION('ref_axis',(-1.,0.,0.));
#2414=DIRECTION('center_axis',(0.,0.,1.));
#2415=DIRECTION('ref_axis',(1.,0.,0.));
#2416=DIRECTION('center_axis',(0.,0.,1.));
#2417=DIRECTION('ref_axis',(1.,0.,0.));
#2418=DIRECTION('center_axis',(0.,0.,-1.));
#2419=DIRECTION('ref_axis',(1.,0.,0.));
#2420=DIRECTION('',(-0.670908116956861,8.21625477953198E-17,-0.74154049019686));
#2421=DIRECTION('center_axis',(0.,0.,1.));
#2422=DIRECTION('ref_axis',(1.,0.,0.));
#2423=DIRECTION('center_axis',(0.,0.,-1.));
#2424=DIRECTION('ref_axis',(-1.,0.,0.));
#2425=DIRECTION('center_axis',(0.,0.,1.));
#2426=DIRECTION('ref_axis',(1.,0.,0.));
#2427=DIRECTION('center_axis',(0.,0.,1.));
#2428=DIRECTION('ref_axis',(1.,0.,0.));
#2429=DIRECTION('center_axis',(0.,0.,1.));
#2430=DIRECTION('ref_axis',(1.,0.,0.));
#2431=DIRECTION('',(0.654028054476354,8.00953363467037E-17,-0.756470292845579));
#2432=DIRECTION('center_axis',(0.,0.,-1.));
#2433=DIRECTION('ref_axis',(-1.,0.,0.));
#2434=DIRECTION('center_axis',(0.,0.,1.));
#2435=DIRECTION('ref_axis',(1.,0.,0.));
#2436=DIRECTION('center_axis',(0.,0.,1.));
#2437=DIRECTION('ref_axis',(1.,0.,0.));
#2438=DIRECTION('center_axis',(0.,0.,1.));
#2439=DIRECTION('ref_axis',(1.,0.,0.));
#2440=DIRECTION('',(0.,0.,-1.));
#2441=DIRECTION('center_axis',(0.,0.,-1.));
#2442=DIRECTION('ref_axis',(1.,0.,0.));
#2443=DIRECTION('',(0.77937567080628,-9.54459920586232E-17,0.626556911824666));
#2444=DIRECTION('center_axis',(0.,0.,1.));
#2445=DIRECTION('ref_axis',(1.,0.,0.));
#2446=DIRECTION('center_axis',(0.,0.,1.));
#2447=DIRECTION('ref_axis',(1.,0.,0.));
#2448=DIRECTION('center_axis',(0.,0.,1.));
#2449=DIRECTION('ref_axis',(1.,0.,0.));
#2450=DIRECTION('center_axis',(0.,0.,-1.));
#2451=DIRECTION('ref_axis',(1.,0.,0.));
#2452=DIRECTION('',(0.549902309986816,-6.7343610376909E-17,0.835228980262996));
#2453=DIRECTION('center_axis',(0.,0.,1.));
#2454=DIRECTION('ref_axis',(1.,0.,0.));
#2455=DIRECTION('center_axis',(0.,0.,1.));
#2456=DIRECTION('ref_axis',(1.,0.,0.));
#2457=DIRECTION('center_axis',(0.,0.,1.));
#2458=DIRECTION('ref_axis',(1.,0.,0.));
#2459=DIRECTION('center_axis',(0.,0.,1.));
#2460=DIRECTION('ref_axis',(1.,0.,0.));
#2461=DIRECTION('center_axis',(0.,0.,1.));
#2462=DIRECTION('ref_axis',(1.,0.,0.));
#2463=DIRECTION('',(0.,0.,-1.));
#2464=DIRECTION('center_axis',(0.,0.,1.));
#2465=DIRECTION('ref_axis',(1.,0.,0.));
#2466=DIRECTION('center_axis',(0.,0.,1.));
#2467=DIRECTION('ref_axis',(1.,0.,0.));
#2468=DIRECTION('center_axis',(0.,0.,1.));
#2469=DIRECTION('ref_axis',(1.,0.,0.));
#2470=DIRECTION('center_axis',(0.,0.,1.));
#2471=DIRECTION('ref_axis',(1.,0.,0.));
#2472=DIRECTION('',(-0.250159656512074,-3.06357222623313E-17,0.968204599376475));
#2473=DIRECTION('center_axis',(0.,0.,1.));
#2474=DIRECTION('ref_axis',(1.,0.,0.));
#2475=DIRECTION('center_axis',(0.,0.,1.));
#2476=DIRECTION('ref_axis',(1.,0.,0.));
#2477=DIRECTION('center_axis',(0.,0.,1.));
#2478=DIRECTION('ref_axis',(1.,0.,0.));
#2479=DIRECTION('center_axis',(0.,0.,1.));
#2480=DIRECTION('ref_axis',(1.,0.,0.));
#2481=DIRECTION('',(0.,0.,1.));
#2482=DIRECTION('center_axis',(0.,0.,1.));
#2483=DIRECTION('ref_axis',(1.,0.,0.));
#2484=DIRECTION('center_axis',(0.,0.,1.));
#2485=DIRECTION('ref_axis',(1.,0.,0.));
#2486=DIRECTION('center_axis',(0.,0.,1.));
#2487=DIRECTION('ref_axis',(1.,0.,0.));
#2488=DIRECTION('center_axis',(0.,0.,1.));
#2489=DIRECTION('ref_axis',(1.,0.,0.));
#2490=DIRECTION('',(0.,0.,1.));
#2491=DIRECTION('center_axis',(0.,0.,1.));
#2492=DIRECTION('ref_axis',(1.,0.,0.));
#2493=DIRECTION('center_axis',(0.,0.,1.));
#2494=DIRECTION('ref_axis',(1.,0.,0.));
#2495=DIRECTION('',(-0.860062224672037,-1.05327245051216E-16,0.510189150896202));
#2496=DIRECTION('center_axis',(0.,0.,1.));
#2497=DIRECTION('ref_axis',(1.,0.,0.));
#2498=DIRECTION('',(0.,0.,1.));
#2499=DIRECTION('axis',(0.,0.,1.));
#2500=DIRECTION('refdir',(1.,0.,0.));
#2501=DIRECTION('center_axis',(0.,0.,1.));
#2502=DIRECTION('ref_axis',(0.983063241079179,0.183266647371803,0.));
#2503=DIRECTION('',(0.,0.,-1.));
#2504=DIRECTION('center_axis',(0.,0.,-1.));
#2505=DIRECTION('ref_axis',(1.,2.64874037426574E-14,0.));
#2506=DIRECTION('center_axis',(0.,0.,1.));
#2507=DIRECTION('ref_axis',(0.835702322852818,-0.549182690530578,0.));
#2508=DIRECTION('',(0.,0.,-1.));
#2509=DIRECTION('center_axis',(0.,0.,1.));
#2510=DIRECTION('ref_axis',(0.835702322852818,-0.549182690530578,0.));
#2511=DIRECTION('',(0.,0.,-1.));
#2512=DIRECTION('center_axis',(0.,0.,1.));
#2513=DIRECTION('ref_axis',(0.835702322852818,-0.549182690530578,0.));
#2514=DIRECTION('',(0.,0.,-1.));
#2515=DIRECTION('center_axis',(0.,0.,1.));
#2516=DIRECTION('ref_axis',(0.835702322852818,-0.549182690530578,0.));
#2517=DIRECTION('',(0.,0.,-1.));
#2518=DIRECTION('center_axis',(0.,0.,1.));
#2519=DIRECTION('ref_axis',(0.835702322852818,-0.549182690530578,0.));
#2520=DIRECTION('',(0.,0.,-1.));
#2521=DIRECTION('center_axis',(0.,0.,1.));
#2522=DIRECTION('ref_axis',(0.835702322852818,-0.549182690530578,0.));
#2523=DIRECTION('',(0.,0.,-1.));
#2524=DIRECTION('center_axis',(0.,0.,1.));
#2525=DIRECTION('ref_axis',(1.,0.,0.));
#2526=DIRECTION('center_axis',(0.,0.,1.));
#2527=DIRECTION('ref_axis',(1.,0.,0.));
#2528=DIRECTION('center_axis',(0.,0.,1.));
#2529=DIRECTION('ref_axis',(1.,0.,0.));
#2530=DIRECTION('center_axis',(0.,0.,1.));
#2531=DIRECTION('ref_axis',(0.637974576266918,-0.770057426454058,0.));
#2532=DIRECTION('center_axis',(0.,0.,1.));
#2533=DIRECTION('ref_axis',(1.,2.64874037426574E-14,0.));
#2534=DIRECTION('center_axis',(0.,0.,1.));
#2535=DIRECTION('ref_axis',(1.,0.,0.));
#2536=DIRECTION('center_axis',(0.,0.,1.));
#2537=DIRECTION('ref_axis',(1.,0.,0.));
#2538=DIRECTION('center_axis',(0.,0.,1.));
#2539=DIRECTION('ref_axis',(1.,0.,0.));
#2540=DIRECTION('center_axis',(0.,0.,1.));
#2541=DIRECTION('ref_axis',(1.,0.,0.));
#2542=DIRECTION('center_axis',(-1.22464679914735E-16,1.,0.));
#2543=DIRECTION('ref_axis',(-1.,-1.22464679914735E-16,0.));
#2544=DIRECTION('center_axis',(0.,0.,1.));
#2545=DIRECTION('ref_axis',(1.,0.,0.));
#2546=DIRECTION('center_axis',(0.,0.,-1.));
#2547=DIRECTION('ref_axis',(-1.,0.,0.));
#2548=DIRECTION('center_axis',(0.,0.,1.));
#2549=DIRECTION('ref_axis',(1.,0.,0.));
#2550=DIRECTION('center_axis',(0.,0.,1.));
#2551=DIRECTION('ref_axis',(1.,0.,0.));
#2552=DIRECTION('center_axis',(0.,0.,1.));
#2553=DIRECTION('ref_axis',(1.,0.,0.));
#2554=DIRECTION('',(0.,0.,-1.));
#2555=DIRECTION('center_axis',(0.,0.,-1.));
#2556=DIRECTION('ref_axis',(1.,0.,0.));
#2557=DIRECTION('',(0.78750500100757,-9.64415478796454E-17,0.616308261658131));
#2558=DIRECTION('center_axis',(0.,0.,1.));
#2559=DIRECTION('ref_axis',(1.,0.,0.));
#2560=DIRECTION('center_axis',(0.,0.,1.));
#2561=DIRECTION('ref_axis',(1.,0.,0.));
#2562=DIRECTION('center_axis',(0.,0.,1.));
#2563=DIRECTION('ref_axis',(1.,0.,0.));
#2564=DIRECTION('center_axis',(0.,0.,1.));
#2565=DIRECTION('ref_axis',(1.,0.,0.));
#2566=DIRECTION('center_axis',(0.,0.,1.));
#2567=DIRECTION('ref_axis',(1.,0.,0.));
#2568=DIRECTION('',(0.,0.,1.));
#2569=DIRECTION('center_axis',(0.,0.,1.));
#2570=DIRECTION('ref_axis',(1.,0.,0.));
#2571=DIRECTION('center_axis',(0.,0.,-1.));
#2572=DIRECTION('ref_axis',(-1.,0.,0.));
#2573=DIRECTION('center_axis',(0.,0.,1.));
#2574=DIRECTION('ref_axis',(1.,0.,0.));
#2575=DIRECTION('center_axis',(0.,0.,1.));
#2576=DIRECTION('ref_axis',(1.,0.,0.));
#2577=DIRECTION('',(0.,0.,-1.));
#2578=DIRECTION('',(0.,0.,1.));
#2579=DIRECTION('',(1.,0.,0.));
#2580=DIRECTION('',(0.,0.,1.));
#2581=DIRECTION('',(1.,0.,0.));
#2582=DIRECTION('',(0.,0.,1.));
#2583=DIRECTION('',(1.,0.,0.));
#2584=DIRECTION('',(0.,0.,1.));
#2585=DIRECTION('',(1.,0.,0.));
#2586=DIRECTION('',(0.,0.,1.));
#2587=DIRECTION('',(1.,0.,0.));
#2588=DIRECTION('',(0.,0.,1.));
#2589=DIRECTION('',(1.,0.,0.));
#2590=DIRECTION('',(0.,0.,1.));
#2591=DIRECTION('',(1.,0.,0.));
#2592=DIRECTION('',(0.,0.,1.));
#2593=DIRECTION('',(1.,0.,0.));
#2594=CARTESIAN_POINT('',(0.,0.,0.));
#2595=CARTESIAN_POINT('',(0.,0.,0.));
#2596=CARTESIAN_POINT('Origin',(10.0021025234003,0.,86.3550920810876));
#2597=CARTESIAN_POINT('',(-11.7021025234003,-1.43309423985764E-15,86.3550920810876));
#2598=CARTESIAN_POINT('Origin',(0.,0.,86.3550920810876));
#2599=CARTESIAN_POINT('',(-10.0021025234003,-1.22490428400259E-15,86.3550920810876));
#2600=CARTESIAN_POINT('Origin',(0.,0.,86.3550920810876));
#2601=CARTESIAN_POINT('Origin',(11.7021025234003,0.,28.3343056886915));
#2602=CARTESIAN_POINT('',(-11.7021025234003,-1.43309423985764E-15,28.3343056886915));
#2603=CARTESIAN_POINT('Origin',(0.,0.,28.3343056886915));
#2604=CARTESIAN_POINT('',(-10.0021025234003,-1.22490428400259E-15,28.3343056886915));
#2605=CARTESIAN_POINT('Origin',(0.,0.,28.3343056886915));
#2606=CARTESIAN_POINT('Origin',(0.,0.,52.3446988848895));
#2607=CARTESIAN_POINT('',(-10.0021025234003,-1.22490428400258E-15,52.3446988848895));
#2608=CARTESIAN_POINT('Origin',(0.,0.,52.3446988848895));
#2609=CARTESIAN_POINT('',(-11.7021025234003,-1.43309423985763E-15,52.3446988848895));
#2610=CARTESIAN_POINT('',(0.,0.,0.));
#2611=CARTESIAN_POINT('Origin',(0.,0.,58.1431215754561));
#2612=CARTESIAN_POINT('',(-1.25945989284257,-1.54239352642412E-16,58.1431215754561));
#2613=CARTESIAN_POINT('Origin',(0.,0.,58.1431215754561));
#2614=CARTESIAN_POINT('Origin',(0.,0.,53.7053570659329));
#2615=CARTESIAN_POINT('',(-10.0021025234003,-1.22490428400259E-15,61.3445102174369));
#2616=CARTESIAN_POINT('Origin',(0.,0.,61.3445102174369));
#2617=CARTESIAN_POINT('',(-10.0021025234003,-1.22490428400259E-15,46.0662039144288));
#2618=CARTESIAN_POINT('',(-10.0021025234003,-1.22490428400258E-15,53.7053570659329));
#2619=CARTESIAN_POINT('Origin',(0.,0.,46.0662039144288));
#2620=CARTESIAN_POINT('Origin',(10.0021025234003,0.,46.0662039144288));
#2621=CARTESIAN_POINT('',(-7.93438181172474,-9.71681528894168E-16,46.0662039144288));
#2622=CARTESIAN_POINT('Origin',(0.,0.,46.0662039144288));
#2623=CARTESIAN_POINT('Origin',(0.,0.,52.1046627449425));
#2624=CARTESIAN_POINT('',(-7.93438181172474,-9.71681528894168E-16,58.1431215754561));
#2625=CARTESIAN_POINT('',(-7.93438181172474,-9.71681528894168E-16,52.1046627449425));
#2626=CARTESIAN_POINT('Origin',(0.,0.,58.1431215754561));
#2627=CARTESIAN_POINT('Origin',(7.93438181172474,0.,58.1431215754561));
#2628=CARTESIAN_POINT('',(-2.72924949802694,-3.34236666183321E-16,58.1431215754561));
#2629=CARTESIAN_POINT('Origin',(0.,0.,58.1431215754561));
#2630=CARTESIAN_POINT('Origin',(0.,0.,57.7133622810548));
#2631=CARTESIAN_POINT('',(-2.72924949802694,-3.34236666183321E-16,57.2836029866534));
#2632=CARTESIAN_POINT('',(-2.72924949802694,-3.34236666183321E-16,57.7133622810548));
#2633=CARTESIAN_POINT('Origin',(0.,0.,57.2836029866534));
#2634=CARTESIAN_POINT('Origin',(2.72924949802694,0.,57.2836029866534));
#2635=CARTESIAN_POINT('',(-3.37974687627927,-4.13899619396367E-16,57.2836029866534));
#2636=CARTESIAN_POINT('Origin',(0.,0.,57.2836029866534));
#2637=CARTESIAN_POINT('Origin',(0.,0.,53.9082407428739));
#2638=CARTESIAN_POINT('',(-3.37974687627927,-4.13899619396367E-16,50.5328784990943));
#2639=CARTESIAN_POINT('',(-3.37974687627927,-4.13899619396367E-16,53.9082407428739));
#2640=CARTESIAN_POINT('Origin',(0.,0.,50.5328784990943));
#2641=CARTESIAN_POINT('Origin',(0.,0.,50.5328784990943));
#2642=CARTESIAN_POINT('',(-2.67974687627927,-3.28174343456053E-16,49.8328784990943));
#2643=CARTESIAN_POINT('Origin',(-2.67974687627927,-3.28174343456053E-16,
50.5328784990943));
#2644=CARTESIAN_POINT('Origin',(0.,0.,49.8328784990943));
#2645=CARTESIAN_POINT('Origin',(2.67974687627927,0.,49.8328784990943));
#2646=CARTESIAN_POINT('',(-1.37433660530134,-1.68307692463333E-16,49.8328784990943));
#2647=CARTESIAN_POINT('Origin',(0.,0.,49.8328784990943));
#2648=CARTESIAN_POINT('Origin',(0.,0.,50.0785885840682));
#2649=CARTESIAN_POINT('',(-1.37433660530134,-1.68307692463333E-16,50.3242986690421));
#2650=CARTESIAN_POINT('',(-1.37433660530134,-1.68307692463333E-16,50.0785885840682));
#2651=CARTESIAN_POINT('Origin',(0.,0.,50.3242986690421));
#2652=CARTESIAN_POINT('Origin',(1.37433660530134,0.,50.3242986690421));
#2653=CARTESIAN_POINT('',(-2.58871463782345,-3.17026109511639E-16,50.3242986690421));
#2654=CARTESIAN_POINT('Origin',(0.,0.,50.3242986690421));
#2655=CARTESIAN_POINT('Origin',(0.,0.,53.0505398104803));
#2656=CARTESIAN_POINT('',(-2.58871463782345,-3.17026109511639E-16,55.7767809519186));
#2657=CARTESIAN_POINT('',(-2.58871463782345,-3.17026109511639E-16,53.0505398104803));
#2658=CARTESIAN_POINT('Origin',(0.,0.,55.7767809519186));
#2659=CARTESIAN_POINT('Origin',(2.58871463782345,0.,55.7767809519186));
#2660=CARTESIAN_POINT('Origin',(10.0021025234003,0.,61.3445102174369));
#2661=CARTESIAN_POINT('',(-1.25945989284257,1.54239352642412E-16,61.3445102174369));
#2662=CARTESIAN_POINT('Origin',(0.,0.,61.3445102174369));
#2663=CARTESIAN_POINT('Origin',(0.,0.,60.205945294667));
#2664=CARTESIAN_POINT('',(-1.25945989284257,-1.54239352642412E-16,60.205945294667));
#2665=CARTESIAN_POINT('',(0.,0.,0.));
#2666=CARTESIAN_POINT('Origin',(0.,0.,14.8197830204816));
#2667=CARTESIAN_POINT('',(-0.544851764215984,-6.67250969056894E-17,16.2795718072011));
#2668=CARTESIAN_POINT('Origin',(0.,0.,16.2795718072011));
#2669=CARTESIAN_POINT('',(-0.544851764215984,-6.67250969056894E-17,13.3599942337622));
#2670=CARTESIAN_POINT('',(-0.544851764215984,-6.67250969056893E-17,14.8197830204816));
#2671=CARTESIAN_POINT('Origin',(0.,0.,13.3599942337622));
#2672=CARTESIAN_POINT('Origin',(1.08970352843197,0.,16.2795718072011));
#2673=CARTESIAN_POINT('',(-1.08970352843197,-1.33450193811379E-16,16.2795718072011));
#2674=CARTESIAN_POINT('Origin',(0.,0.,16.2795718072011));
#2675=CARTESIAN_POINT('Origin',(0.,0.,32.1916732743837));
#2676=CARTESIAN_POINT('',(-1.08970352843197,-1.33450193811379E-16,48.1037747415664));
#2677=CARTESIAN_POINT('Origin',(0.,0.,48.1037747415664));
#2678=CARTESIAN_POINT('',(-1.08970352843197,-1.33450193811379E-16,32.1916732743837));
#2679=CARTESIAN_POINT('Origin',(0.625182919763592,0.,48.1037747415664));
#2680=CARTESIAN_POINT('',(-0.625182919763592,-7.65628261570079E-17,48.1037747415664));
#2681=CARTESIAN_POINT('Origin',(0.,0.,48.1037747415664));
#2682=CARTESIAN_POINT('Origin',(0.,0.,49.4350798260675));
#2683=CARTESIAN_POINT('',(-0.625182919763592,-7.65628261570079E-17,50.7663849105686));
#2684=CARTESIAN_POINT('Origin',(0.,0.,50.7663849105686));
#2685=CARTESIAN_POINT('',(-0.625182919763592,-7.6562826157008E-17,49.4350798260675));
#2686=CARTESIAN_POINT('Origin',(0.,0.,52.6508016020046));
#2687=CARTESIAN_POINT('',(-1.2157171769455E-16,-2.97764829882954E-32,54.6362184222534));
#2688=CARTESIAN_POINT('Origin',(0.,0.,52.6508016020046));
#2689=CARTESIAN_POINT('Origin',(0.,0.,11.4508016020046));
#2690=CARTESIAN_POINT('',(-1.2157171769455E-16,-1.3684555315672E-47,9.4653847817558));
#2691=CARTESIAN_POINT('Origin',(0.,0.,11.4508016020046));
#2692=CARTESIAN_POINT('',(0.,0.,0.));
#2693=CARTESIAN_POINT('Origin',(0.,0.,61.3445102174369));
#2694=CARTESIAN_POINT('',(-8.93704988738917,-1.09447295384114E-15,61.3445102174369));
#2695=CARTESIAN_POINT('Origin',(0.,0.,61.3445102174369));
#2696=CARTESIAN_POINT('',(-1.25945989284257,1.54239352642412E-16,61.3445102174369));
#2697=CARTESIAN_POINT('Origin',(0.,0.,61.3445102174369));
#2698=CARTESIAN_POINT('Origin',(0.,0.,61.8066396156573));
#2699=CARTESIAN_POINT('',(-8.93704988738917,-1.09447295384114E-15,62.2687690138778));
#2700=CARTESIAN_POINT('Origin',(0.,0.,62.2687690138778));
#2701=CARTESIAN_POINT('',(-8.93704988738917,-1.09447295384114E-15,61.8066396156573));
#2702=CARTESIAN_POINT('Origin',(1.25945989284257,0.,62.2687690138778));
#2703=CARTESIAN_POINT('',(-1.25945989284257,-1.54239352642412E-16,62.2687690138778));
#2704=CARTESIAN_POINT('Origin',(0.,0.,62.2687690138778));
#2705=CARTESIAN_POINT('Origin',(0.,0.,60.205945294667));
#2706=CARTESIAN_POINT('',(-1.25945989284257,-1.54239352642412E-16,60.205945294667));
#2707=CARTESIAN_POINT('',(0.,0.,0.));
#2708=CARTESIAN_POINT('Origin',(0.,0.,27.4843056886915));
#2709=CARTESIAN_POINT('',(-8.2210249646156,-1.0067851908627E-15,26.6343056886915));
#2710=CARTESIAN_POINT('Origin',(0.,0.,26.6343056886915));
#2711=CARTESIAN_POINT('',(-8.2210249646156,-1.0067851908627E-15,28.3343056886915));
#2712=CARTESIAN_POINT('',(-8.2210249646156,-1.0067851908627E-15,27.4843056886915));
#2713=CARTESIAN_POINT('Origin',(0.,0.,28.3343056886915));
#2714=CARTESIAN_POINT('Origin',(13.263882223741,0.,26.6343056886915));
#2715=CARTESIAN_POINT('',(-13.263882223741,-1.62435709095719E-15,26.6343056886915));
#2716=CARTESIAN_POINT('Origin',(0.,0.,26.6343056886915));
#2717=CARTESIAN_POINT('Origin',(0.,0.,31.7196089913165));
#2718=CARTESIAN_POINT('',(-13.263882223741,-1.62435709095719E-15,36.8049122939414));
#2719=CARTESIAN_POINT('Origin',(0.,0.,36.8049122939414));
#2720=CARTESIAN_POINT('',(-13.263882223741,-1.62435709095719E-15,31.7196089913165));
#2721=CARTESIAN_POINT('Origin',(11.7021025234003,0.,36.8049122939414));
#2722=CARTESIAN_POINT('',(-11.7021025234003,-1.43309423985764E-15,36.8049122939414));
#2723=CARTESIAN_POINT('Origin',(0.,0.,36.8049122939414));
#2724=CARTESIAN_POINT('Origin',(0.,0.,32.5696089913164));
#2725=CARTESIAN_POINT('',(-11.7021025234003,-1.43309423985764E-15,28.3343056886915));
#2726=CARTESIAN_POINT('Origin',(0.,0.,28.3343056886915));
#2727=CARTESIAN_POINT('',(-11.7021025234003,-1.43309423985763E-15,32.5696089913164));
#2728=CARTESIAN_POINT('Origin',(8.2210249646156,0.,28.3343056886915));
#2729=CARTESIAN_POINT('',(0.,0.,0.));
#2730=CARTESIAN_POINT('Origin',(0.,0.,-1.10921167016993));
#2731=CARTESIAN_POINT('',(-1.14737960344596,0.741266514552076,0.454399650883576));
#2732=CARTESIAN_POINT('',(-1.14737960344596,0.741266514552078,0.335993717254283));
#2733=CARTESIAN_POINT('',(-1.14737960344596,0.741266514552077,-1.10921167016993));
#2734=CARTESIAN_POINT('',(-0.793737169645199,-1.11172717225209,4.50645841770791E-5));
#2735=CARTESIAN_POINT('Ctrl Pts',(-0.793737169645199,-1.11172717225209,
4.50645841774122E-5));
#2736=CARTESIAN_POINT('Ctrl Pts',(-0.751639642335613,-1.14178344236023,
0.0036785650865398));
#2737=CARTESIAN_POINT('Ctrl Pts',(-0.70774020306432,-1.16951088815659,0.00731206558890195));
#2738=CARTESIAN_POINT('Ctrl Pts',(-0.662329724218108,-1.19468629205209,
0.0109455660912643));
#2739=CARTESIAN_POINT('Ctrl Pts',(-0.616977478597539,-1.21982941165962,
0.0145744070863938));
#2740=CARTESIAN_POINT('Ctrl Pts',(-0.570118503567981,-1.24242669896913,
0.0182032480815238));
#2741=CARTESIAN_POINT('Ctrl Pts',(-0.52207319003199,-1.26229773993691,0.0218320890766532));
#2742=CARTESIAN_POINT('Ctrl Pts',(-0.474068808551045,-1.2821518518333,0.0254578384920127));
#2743=CARTESIAN_POINT('Ctrl Pts',(-0.424880595233744,-1.29928410516619,
0.0290835879073719));
#2744=CARTESIAN_POINT('Ctrl Pts',(-0.374851798930883,-1.31356085844482,
0.0327093373227314));
#2745=CARTESIAN_POINT('Ctrl Pts',(-0.324844095785002,-1.32783159235419,
0.0363335580484712));
#2746=CARTESIAN_POINT('Ctrl Pts',(-0.273997040078241,-1.33924906128545,
0.039957778774211));
#2747=CARTESIAN_POINT('Ctrl Pts',(-0.222669546158888,-1.34772930264701,
0.0435819994999509));
#2748=CARTESIAN_POINT('Ctrl Pts',(-0.171305410096995,-1.35621559796112,
0.0472088075176525));
#2749=CARTESIAN_POINT('Ctrl Pts',(-0.119460693090967,-1.36176037993733,
0.050835615535354));
#2750=CARTESIAN_POINT('Ctrl Pts',(-0.0675032006527575,-1.36433108808003,
0.0544624235530555));
#2751=CARTESIAN_POINT('Ctrl Pts',(-0.0155290642017095,-1.36690261972089,
0.0580903933789271));
#2752=CARTESIAN_POINT('Ctrl Pts',(0.0365573687379424,-1.36649817889123,
0.0617183632047989));
#2753=CARTESIAN_POINT('Ctrl Pts',(0.088388047322021,-1.36313739332857,0.0653463330306705));
#2754=CARTESIAN_POINT('Ctrl Pts',(0.140314932876691,-1.35977036954934,0.068981037014687));
#2755=CARTESIAN_POINT('Ctrl Pts',(0.191984568102908,-1.35343610419073,0.0726157409987032));
#2756=CARTESIAN_POINT('Ctrl Pts',(0.243035214301144,-1.34420604246879,0.0762504449827197));
#2757=CARTESIAN_POINT('Ctrl Pts',(0.286596093508279,-1.3363301460074,0.0793518925253544));
#2758=CARTESIAN_POINT('Ctrl Pts',(0.329706251292679,-1.32634675090387,0.0824533400679891));
#2759=CARTESIAN_POINT('Ctrl Pts',(0.372150158132393,-1.31432882483876,0.0855547876106237));
#2760=CARTESIAN_POINT('Ctrl Pts',(0.422553436740067,-1.30005721506368,0.0892378398133543));
#2761=CARTESIAN_POINT('Ctrl Pts',(0.472236728814164,-1.28285315030033,0.0929208920160846));
#2762=CARTESIAN_POINT('Ctrl Pts',(0.520836570594336,-1.26280848378982,0.0966039442188151));
#2763=CARTESIAN_POINT('Ctrl Pts',(0.569352750610994,-1.24279832299142,0.10028065626423));
#2764=CARTESIAN_POINT('Ctrl Pts',(0.61678869076564,-1.21995746573567,0.103957368309646));
#2765=CARTESIAN_POINT('Ctrl Pts',(0.662796534801183,-1.19442737470955,0.107634080355061));
#2766=CARTESIAN_POINT('Ctrl Pts',(0.708760648998604,-1.16892154969221,0.111307297735035));
#2767=CARTESIAN_POINT('Ctrl Pts',(0.753298890590591,-1.14073181236285,0.114980515115009));
#2768=CARTESIAN_POINT('Ctrl Pts',(0.796085668064992,-1.11004666978534,0.118653732494983));
#2769=CARTESIAN_POINT('Ctrl Pts',(0.838849036797168,-1.07937831511837,0.122324940249464));
#2770=CARTESIAN_POINT('Ctrl Pts',(0.879862407211625,-1.04621757228296,0.125996148003945));
#2771=CARTESIAN_POINT('Ctrl Pts',(0.918829042873192,-1.01079631477995,0.129667355758426));
#2772=CARTESIAN_POINT('Ctrl Pts',(0.957790077042176,-0.975380149117903,
0.133338035773145));
#2773=CARTESIAN_POINT('Ctrl Pts',(0.994704566209091,-0.937704474229589,
0.137008715787865));
#2774=CARTESIAN_POINT('Ctrl Pts',(1.02931060115345,-0.898039913563496,0.140679395802584));
#2775=CARTESIAN_POINT('Ctrl Pts',(1.06394993909219,-0.858337181848816,0.144353608283133));
#2776=CARTESIAN_POINT('Ctrl Pts',(1.09627603522514,-0.816642146342524,0.148027820763682));
#2777=CARTESIAN_POINT('Ctrl Pts',(1.12606657452244,-0.773259380637117,0.15170203324423));
#2778=CARTESIAN_POINT('Ctrl Pts',(1.15587257497474,-0.729854099472749,0.15537815262442));
#2779=CARTESIAN_POINT('Ctrl Pts',(1.18314012000445,-0.684759800914628,0.159054272004609));
#2780=CARTESIAN_POINT('Ctrl Pts',(1.20769149326283,-0.63830812081673,0.162730391384798));
#2781=CARTESIAN_POINT('Ctrl Pts',(1.23228776877378,-0.591771484775637,0.166413234056558));
#2782=CARTESIAN_POINT('Ctrl Pts',(1.254157732108,-0.543872997364555,0.170096076728318));
#2783=CARTESIAN_POINT('Ctrl Pts',(1.27317128162862,-0.494965541867454,0.173778919400078));
#2784=CARTESIAN_POINT('Ctrl Pts',(1.28377240174473,-0.467696892753009,0.175832310719237));
#2785=CARTESIAN_POINT('Ctrl Pts',(1.29348643851001,-0.440114891305328,0.177885702038397));
#2786=CARTESIAN_POINT('Ctrl Pts',(1.30229766419691,-0.412282419983284,0.179939093357556));
#2787=CARTESIAN_POINT('Ctrl Pts',(1.3180543625256,-0.362510927350304,0.183611075975687));
#2788=CARTESIAN_POINT('Ctrl Pts',(1.33098780187201,-0.311727064905966,0.187283058593818));
#2789=CARTESIAN_POINT('Ctrl Pts',(1.34097323626866,-0.260282115426988,0.190955041211949));
#2790=CARTESIAN_POINT('Ctrl Pts',(1.35094057822144,-0.208930378203374,0.194620370625344));
#2791=CARTESIAN_POINT('Ctrl Pts',(1.3579704104302,-0.156920454413018,0.198285700038739));
#2792=CARTESIAN_POINT('Ctrl Pts',(1.36198789621833,-0.104618213303267,0.201951029452135));
#2793=CARTESIAN_POINT('Ctrl Pts',(1.36600135074658,-0.0523684537546225,
0.205612680969411));
#2794=CARTESIAN_POINT('Ctrl Pts',(1.36700840358335,0.000172508177129028,
0.209274332486688));
#2795=CARTESIAN_POINT('Ctrl Pts',(1.36498569854959,0.0526311956457186,0.212935984003965));
#2796=CARTESIAN_POINT('Ctrl Pts',(1.36296419249614,0.105058787658907,0.216595465037629));
#2797=CARTESIAN_POINT('Ctrl Pts',(1.35791650798661,0.157403665011107,0.220254946071294));
#2798=CARTESIAN_POINT('Ctrl Pts',(1.34987137383988,0.209292317316323,0.223914427104958));
#2799=CARTESIAN_POINT('Ctrl Pts',(1.34182770485348,0.261171519785902,0.227573241682804));
#2800=CARTESIAN_POINT('Ctrl Pts',(1.33078775312727,0.312594130645045,0.231232056260649));
#2801=CARTESIAN_POINT('Ctrl Pts',(1.31683179740051,0.363194186840785,0.234890870838494));
#2802=CARTESIAN_POINT('Ctrl Pts',(1.30286281544566,0.413841472182751,0.238553100485446));
#2803=CARTESIAN_POINT('Ctrl Pts',(1.2859725378804,0.463664149814199,0.242215330132398));
#2804=CARTESIAN_POINT('Ctrl Pts',(1.26629142338985,0.512310483056241,0.24587755977935));
#2805=CARTESIAN_POINT('Ctrl Pts',(1.24660050841667,0.560981040411392,0.249541613084105));
#2806=CARTESIAN_POINT('Ctrl Pts',(1.22411621856117,0.608473599297943,0.25320566638886));
#2807=CARTESIAN_POINT('Ctrl Pts',(1.19901620077949,0.654458669641039,0.256869719693615));
#2808=CARTESIAN_POINT('Ctrl Pts',(1.17387005003326,0.700528258952944,0.260540507401615));
#2809=CARTESIAN_POINT('Ctrl Pts',(1.1460988579627,0.74508437064621,0.264211295109616));
#2810=CARTESIAN_POINT('Ctrl Pts',(1.11592426213602,0.787825514423194,0.267882082817616));
#2811=CARTESIAN_POINT('Ctrl Pts',(1.09827463386285,0.812825527810852,0.270029188246571));
#2812=CARTESIAN_POINT('Ctrl Pts',(1.0798035203546,0.837205186230783,0.272176293675525));
#2813=CARTESIAN_POINT('Ctrl Pts',(1.06056136792303,0.860909742580046,0.274323399104479));
#2814=CARTESIAN_POINT('Ctrl Pts',(1.02759784932718,0.901517755992458,0.278001581677153));
#2815=CARTESIAN_POINT('Ctrl Pts',(0.992229539636963,0.940315040623115,0.281679764249827));
#2816=CARTESIAN_POINT('Ctrl Pts',(0.954682800137662,0.977003966788935,0.285357946822501));
#2817=CARTESIAN_POINT('Ctrl Pts',(0.917202768032331,1.01362770959437,0.289029594554142));
#2818=CARTESIAN_POINT('Ctrl Pts',(0.877552365838462,1.04815015433973,0.292701242285782));
#2819=CARTESIAN_POINT('Ctrl Pts',(0.835997481287777,1.08030746145738,0.296372890017422));
#2820=CARTESIAN_POINT('Ctrl Pts',(0.794483456349179,1.11243314930551,0.300040927533232));
#2821=CARTESIAN_POINT('Ctrl Pts',(0.751069080026469,1.1421979789467,0.303708965049042));
#2822=CARTESIAN_POINT('Ctrl Pts',(0.706054797570703,1.16937702338784,0.307377002564852));
#2823=CARTESIAN_POINT('Ctrl Pts',(0.661066469187005,1.19654039709426,0.311042925185015));
#2824=CARTESIAN_POINT('Ctrl Pts',(0.614480521023724,1.22112066376083,0.314708847805177));
#2825=CARTESIAN_POINT('Ctrl Pts',(0.566625972166103,1.24293644554612,0.31837477042534));
#2826=CARTESIAN_POINT('Ctrl Pts',(0.51877955420565,1.26474852064349,0.322040070173893));
#2827=CARTESIAN_POINT('Ctrl Pts',(0.469665451480756,1.2837968219978,0.325705369922446));
#2828=CARTESIAN_POINT('Ctrl Pts',(0.419634648089527,1.29994721512944,0.329370669670999));
#2829=CARTESIAN_POINT('Ctrl Pts',(0.369557020317372,1.31611272359221,0.33303939981403));
#2830=CARTESIAN_POINT('Ctrl Pts',(0.318561489935458,1.32937474308056,0.336708129957061));
#2831=CARTESIAN_POINT('Ctrl Pts',(0.267014692991089,1.33964889195896,0.340376860100091));
#2832=CARTESIAN_POINT('Ctrl Pts',(0.215442020405072,1.3499281982906,0.344047431885127));
#2833=CARTESIAN_POINT('Ctrl Pts',(0.163318061560322,1.35721657132989,0.347718003670162));
#2834=CARTESIAN_POINT('Ctrl Pts',(0.111016790111677,1.36148127872303,0.351388575455198));
#2835=CARTESIAN_POINT('Ctrl Pts',(0.0586202528237817,1.36575375420512,0.355065833121703));
#2836=CARTESIAN_POINT('Ctrl Pts',(0.00604629471542903,1.36699155515212,
0.358743090788209));
#2837=CARTESIAN_POINT('Ctrl Pts',(-0.046330323551458,1.36521408618561,0.362420348454715));
#2838=CARTESIAN_POINT('Ctrl Pts',(-0.0761814151132315,1.36420105039554,
0.364516133920278));
#2839=CARTESIAN_POINT('Ctrl Pts',(-0.10596847410221,1.36220954607447,0.366611919385841));
#2840=CARTESIAN_POINT('Ctrl Pts',(-0.135623318953185,1.35925064478783,0.368707704851404));
#2841=CARTESIAN_POINT('Ctrl Pts',(-0.187642818708641,1.35406024283056,0.372384058987169));
#2842=CARTESIAN_POINT('Ctrl Pts',(-0.23947307154391,1.34586842646892,0.376060413122934));
#2843=CARTESIAN_POINT('Ctrl Pts',(-0.290741487431388,1.33470048605902,0.379736767258699));
#2844=CARTESIAN_POINT('Ctrl Pts',(-0.341937330532648,1.32354835437926,0.383407917347135));
#2845=CARTESIAN_POINT('Ctrl Pts',(-0.392572392128989,1.30942855401121,0.387079067435571));
#2846=CARTESIAN_POINT('Ctrl Pts',(-0.442280156726634,1.29241799080865,0.390750217524007));
#2847=CARTESIAN_POINT('Ctrl Pts',(-0.491937793461506,1.27542458193167,0.394417665436146));
#2848=CARTESIAN_POINT('Ctrl Pts',(-0.540669480756072,1.25554635847026,0.398085113348285));
#2849=CARTESIAN_POINT('Ctrl Pts',(-0.588122222418167,1.23291047992055,0.401752561260424));
#2850=CARTESIAN_POINT('Ctrl Pts',(-0.63554642529022,1.21028821492746,0.405417803514423));
#2851=CARTESIAN_POINT('Ctrl Pts',(-0.681692724534928,1.18491181371754,0.409083045768422));
#2852=CARTESIAN_POINT('Ctrl Pts',(-0.72622880467367,1.15695623221549,0.41274828802242));
#2853=CARTESIAN_POINT('Ctrl Pts',(-0.770780158134974,1.12899106355146,0.41641478724441));
#2854=CARTESIAN_POINT('Ctrl Pts',(-0.813719727493361,1.09844522153416,0.4200812864664));
#2855=CARTESIAN_POINT('Ctrl Pts',(-0.854742110151995,1.06553832644955,0.42374778568839));
#2856=CARTESIAN_POINT('Ctrl Pts',(-0.895769796412266,1.03262717697865,0.427414758935778));
#2857=CARTESIAN_POINT('Ctrl Pts',(-0.934879393335804,0.997354714589682,
0.431081732183166));
#2858=CARTESIAN_POINT('Ctrl Pts',(-0.971799154517271,0.959980418175037,
0.434748705430555));
#2859=CARTESIAN_POINT('Ctrl Pts',(-1.00877133198009,0.922553060159411,0.438420884808625));
#2860=CARTESIAN_POINT('Ctrl Pts',(-1.04354709922193,0.88301830310746,0.442093064186694));
#2861=CARTESIAN_POINT('Ctrl Pts',(-1.07589314086733,0.841670927046092,0.445765243564764));
#2862=CARTESIAN_POINT('Ctrl Pts',(-1.10124492518607,0.809264187094878,0.448643379337701));
#2863=CARTESIAN_POINT('Ctrl Pts',(-1.12510489750646,0.775744725514016,0.451521515110639));
#2864=CARTESIAN_POINT('Ctrl Pts',(-1.14737960344596,0.741266514552077,0.454399650883576));
#2865=CARTESIAN_POINT('',(0.79376424639115,-1.11170783983522,0.));
#2866=CARTESIAN_POINT('Origin',(0.,0.,0.));
#2867=CARTESIAN_POINT('Ctrl Pts',(0.793764246391152,-1.11170783983522,-4.44089209850063E-16));
#2868=CARTESIAN_POINT('Ctrl Pts',(0.839547624132048,-1.07901830844257,0.00393267940612148));
#2869=CARTESIAN_POINT('Ctrl Pts',(0.88334665467536,-1.04346915171738,0.00786535881224336));
#2870=CARTESIAN_POINT('Ctrl Pts',(0.924804470391501,-1.00533212996696,0.0117980382183653));
#2871=CARTESIAN_POINT('Ctrl Pts',(0.964439482492348,-0.968871904254196,
0.0155578068689291));
#2872=CARTESIAN_POINT('Ctrl Pts',(1.00193447662138,-0.930047025035295,0.0193175755194929));
#2873=CARTESIAN_POINT('Ctrl Pts',(1.03701191980893,-0.889135691654659,0.0230773441700567));
#2874=CARTESIAN_POINT('Ctrl Pts',(1.07208184091284,-0.848233131389829,0.0268363065676081));
#2875=CARTESIAN_POINT('Ctrl Pts',(1.10473491471357,-0.805245385353481,0.0305952689651596));
#2876=CARTESIAN_POINT('Ctrl Pts',(1.13473279690904,-0.76048502918794,0.034354231362711));
#2877=CARTESIAN_POINT('Ctrl Pts',(1.16473383991346,-0.715719956724978,0.0381135898336224));
#2878=CARTESIAN_POINT('Ctrl Pts',(1.19207885790094,-0.669182319737291,0.0418729483045338));
#2879=CARTESIAN_POINT('Ctrl Pts',(1.21657301646592,-0.621213405849402,0.0456323067754452));
#2880=CARTESIAN_POINT('Ctrl Pts',(1.24107759069276,-0.573224094119078,0.0493932638400193));
#2881=CARTESIAN_POINT('Ctrl Pts',(1.26272867202181,-0.52380274333007,0.0531542209045935));
#2882=CARTESIAN_POINT('Ctrl Pts',(1.28137842533247,-0.473313142742192,0.0569151779691677));
#2883=CARTESIAN_POINT('Ctrl Pts',(1.30005661343255,-0.422746561985347,0.0606818692662755));
#2884=CARTESIAN_POINT('Ctrl Pts',(1.31572416930455,-0.371108952170183,0.0644485605633832));
#2885=CARTESIAN_POINT('Ctrl Pts',(1.32828263625582,-0.318780862382442,0.068215251860491));
#2886=CARTESIAN_POINT('Ctrl Pts',(1.34085194875564,-0.266407581820977,0.0719851960891464));
#2887=CARTESIAN_POINT('Ctrl Pts',(1.35030673650858,-0.213343126544116,0.0757551403178016));
#2888=CARTESIAN_POINT('Ctrl Pts',(1.35659995290541,-0.159976772617293,0.079525084546457));
#2889=CARTESIAN_POINT('Ctrl Pts',(1.36290556532907,-0.106505300621519,0.0833024546010909));
#2890=CARTESIAN_POINT('Ctrl Pts',(1.3660371439318,-0.0527312425025266,0.087079824655725));
#2891=CARTESIAN_POINT('Ctrl Pts',(1.36599966715517,0.000953588993072139,
0.0908571947103589));
#2892=CARTESIAN_POINT('Ctrl Pts',(1.36598800253573,0.0176629537032467,0.0920328983892155));
#2893=CARTESIAN_POINT('Ctrl Pts',(1.36566971183152,0.0343637026982444,0.0932086020680719));
#2894=CARTESIAN_POINT('Ctrl Pts',(1.36504596856042,0.0510441349907324,0.0943843057469285));
#2895=CARTESIAN_POINT('Ctrl Pts',(1.36311507457556,0.102680998858287,0.0980238787357558));
#2896=CARTESIAN_POINT('Ctrl Pts',(1.35824494995059,0.154340769049966,0.101663451724583));
#2897=CARTESIAN_POINT('Ctrl Pts',(1.35043002218929,0.205656886998317,0.10530302471341));
#2898=CARTESIAN_POINT('Ctrl Pts',(1.34263095596918,0.256868851364768,0.108935210655466));
#2899=CARTESIAN_POINT('Ctrl Pts',(1.33189901875094,0.307738009171175,0.112567396597523));
#2900=CARTESIAN_POINT('Ctrl Pts',(1.31828056759875,0.357899909320372,0.116199582539579));
#2901=CARTESIAN_POINT('Ctrl Pts',(1.3046775273593,0.408005045256218,0.119827658227097));
#2902=CARTESIAN_POINT('Ctrl Pts',(1.28819457884667,0.457403980420958,0.123455733914616));
#2903=CARTESIAN_POINT('Ctrl Pts',(1.2689292619985,0.505741562503954,0.127083809602134));
#2904=CARTESIAN_POINT('Ctrl Pts',(1.24967747407379,0.554045199884493,0.130709337500863));
#2905=CARTESIAN_POINT('Ctrl Pts',(1.22764738884494,0.601288450906808,0.134334865399592));
#2906=CARTESIAN_POINT('Ctrl Pts',(1.20298583332618,0.647132973056167,0.137960393298322));
#2907=CARTESIAN_POINT('Ctrl Pts',(1.17833100864943,0.692964982927643,0.141584931687064));
#2908=CARTESIAN_POINT('Ctrl Pts',(1.15104639821546,0.737398537781149,0.145209470075805));
#2909=CARTESIAN_POINT('Ctrl Pts',(1.12132509524405,0.780119241382957,0.148834008464547));
#2910=CARTESIAN_POINT('Ctrl Pts',(1.09157774953995,0.822877378197753,0.152461722786877));
#2911=CARTESIAN_POINT('Ctrl Pts',(1.05938976027312,0.863919213687103,0.156089437109208));
#2912=CARTESIAN_POINT('Ctrl Pts',(1.02499693519614,0.902960288627645,0.159717151431538));
#2913=CARTESIAN_POINT('Ctrl Pts',(0.990588653942779,0.942018908673566,0.163346496052987));
#2914=CARTESIAN_POINT('Ctrl Pts',(0.953973950157304,0.979074586295714,0.166975840674436));
#2915=CARTESIAN_POINT('Ctrl Pts',(0.915425782563449,1.01387949807563,0.170605185295885));
#2916=CARTESIAN_POINT('Ctrl Pts',(0.876805015732143,1.04874995927625,0.174241365200783));
#2917=CARTESIAN_POINT('Ctrl Pts',(0.836243944415294,1.08136084783297,0.177877545105682));
#2918=CARTESIAN_POINT('Ctrl Pts',(0.794047693405854,1.11150540286444,0.18151372501058));
#2919=CARTESIAN_POINT('Ctrl Pts',(0.765984449461231,1.13155348726087,0.183932020505004));
#2920=CARTESIAN_POINT('Ctrl Pts',(0.737198571536647,1.15051157425271,0.186350315999428));
#2921=CARTESIAN_POINT('Ctrl Pts',(0.707785740498224,1.16833015263126,0.188768611493852));
#2922=CARTESIAN_POINT('Ctrl Pts',(0.662990831832107,1.19546734285903,0.192451607042933));
#2923=CARTESIAN_POINT('Ctrl Pts',(0.616540497489185,1.22008065146032,0.196134602592014));
#2924=CARTESIAN_POINT('Ctrl Pts',(0.568749283224068,1.24196628490153,0.199817598141095));
#2925=CARTESIAN_POINT('Ctrl Pts',(0.521042871503823,1.26381308364392,0.203494058443058));
#2926=CARTESIAN_POINT('Ctrl Pts',(0.472000783491401,1.28294159078561,0.20717051874502));
#2927=CARTESIAN_POINT('Ctrl Pts',(0.421963296418883,1.29919320213558,0.210846979046983));
#2928=CARTESIAN_POINT('Ctrl Pts',(0.371975013053495,1.31542883267653,0.214519824149891));
#2929=CARTESIAN_POINT('Ctrl Pts',(0.320993775526985,1.32879300680675,0.218192669252799));
#2930=CARTESIAN_POINT('Ctrl Pts',(0.269379203383589,1.33917543465538,0.221865514355707));
#2931=CARTESIAN_POINT('Ctrl Pts',(0.217794559408266,1.34955184236217,0.22553622979792));
#2932=CARTESIAN_POINT('Ctrl Pts',(0.165577831743621,1.35694982551169,0.229206945240134));
#2933=CARTESIAN_POINT('Ctrl Pts',(0.113100803751644,1.36130973998967,0.232877660682347));
#2934=CARTESIAN_POINT('Ctrl Pts',(0.0606330314821481,1.36566888548053,0.236547728696062));
#2935=CARTESIAN_POINT('Ctrl Pts',(0.00790558248072019,1.36699098290877,
0.240217796709777));
#2936=CARTESIAN_POINT('Ctrl Pts',(-0.0447050425036199,1.36526827370109,
0.243887864723492));
#2937=CARTESIAN_POINT('Ctrl Pts',(-0.0973637415889933,1.36354399033045,
0.247561286341551));
#2938=CARTESIAN_POINT('Ctrl Pts',(-0.149904868266707,1.35876936192454,0.251234707959611));
#2939=CARTESIAN_POINT('Ctrl Pts',(-0.201953983831821,1.35098874474011,0.25490812957767));
#2940=CARTESIAN_POINT('Ctrl Pts',(-0.254028665796359,1.34320430573537,0.258583355571525));
#2941=CARTESIAN_POINT('Ctrl Pts',(-0.305610331150917,1.33241104487945,0.26225858156538));
#2942=CARTESIAN_POINT('Ctrl Pts',(-0.356335033438439,1.31870441871726,0.265933807559235));
#2943=CARTESIAN_POINT('Ctrl Pts',(-0.407150432714315,1.30497328477765,0.26961560494561));
#2944=CARTESIAN_POINT('Ctrl Pts',(-0.457105301754811,1.28831855360352,0.273297402331984));
#2945=CARTESIAN_POINT('Ctrl Pts',(-0.505852515199843,1.26888503532274,0.276979199718359));
#2946=CARTESIAN_POINT('Ctrl Pts',(-0.533099309290899,1.25802285400733,0.279037105559165));
#2947=CARTESIAN_POINT('Ctrl Pts',(-0.559969194260518,1.24629339880498,0.281095011399971));
#2948=CARTESIAN_POINT('Ctrl Pts',(-0.586404959992857,1.23372818031193,0.283152917240777));
#2949=CARTESIAN_POINT('Ctrl Pts',(-0.633713951483963,1.21124168149852,0.2868357101244));
#2950=CARTESIAN_POINT('Ctrl Pts',(-0.67982354190126,1.18598452557416,0.290518503008023));
#2951=CARTESIAN_POINT('Ctrl Pts',(-0.724390781783443,1.15810793765831,0.294201295891646));
#2952=CARTESIAN_POINT('Ctrl Pts',(-0.768884467149523,1.13027735772814,0.297878010632463));
#2953=CARTESIAN_POINT('Ctrl Pts',(-0.811840401668115,1.09983620262544,0.30155472537328));
#2954=CARTESIAN_POINT('Ctrl Pts',(-0.852939234293832,1.06698203480764,0.305231440114097));
#2955=CARTESIAN_POINT('Ctrl Pts',(-0.89399780078697,1.03416005550208,0.308904552633786));
#2956=CARTESIAN_POINT('Ctrl Pts',(-0.933202455006571,0.998930080160931,
0.312577665153476));
#2957=CARTESIAN_POINT('Ctrl Pts',(-0.970263678560064,0.961532315664478,
0.316250777673165));
#2958=CARTESIAN_POINT('Ctrl Pts',(-1.0073116793192,0.924147894034291,0.319922579690749));
#2959=CARTESIAN_POINT('Ctrl Pts',(-1.04221738145856,0.88459758727491,0.323594381708332));
#2960=CARTESIAN_POINT('Ctrl Pts',(-1.07472681225964,0.843159699588541,0.327266183725916));
#2961=CARTESIAN_POINT('Ctrl Pts',(-1.10048411489069,0.810328358429109,0.330175361568705));
#2962=CARTESIAN_POINT('Ctrl Pts',(-1.12473780846742,0.776312929348634,0.333084539411494));
#2963=CARTESIAN_POINT('Ctrl Pts',(-1.14737960344596,0.741266514552078,0.335993717254284));
#2964=CARTESIAN_POINT('Origin',(0.,0.,-1.10921167016993));
#2965=CARTESIAN_POINT('',(-1.14737959575237,0.741266526460718,1.05477007217181));
#2966=CARTESIAN_POINT('',(-1.14885860607148,0.742234466194312,0.935969339060826));
#2967=CARTESIAN_POINT('',(-1.14737960344596,0.741266514552077,-1.10921167016993));
#2968=CARTESIAN_POINT('',(-1.36599999643447,9.5954861566352E-5,0.509307464475418));
#2969=CARTESIAN_POINT('Ctrl Pts',(-1.14737959575237,0.741266526460718,1.05477007217181));
#2970=CARTESIAN_POINT('Ctrl Pts',(-1.12470332541913,0.776366303611523,1.05162393080854));
#2971=CARTESIAN_POINT('Ctrl Pts',(-1.10042580611056,0.810411025106853,1.04845578440971));
#2972=CARTESIAN_POINT('Ctrl Pts',(-1.03892990164795,0.888776365247056,1.04093215917889));
#2973=CARTESIAN_POINT('Ctrl Pts',(-1.00038150994656,0.931953319766969,1.036593838144));
#2974=CARTESIAN_POINT('Ctrl Pts',(-0.95058246780969,0.9810686879414,1.03152583234021));
#2975=CARTESIAN_POINT('Ctrl Pts',(-0.941842921853207,0.989461841099333,
1.03065475304995));
#2976=CARTESIAN_POINT('Ctrl Pts',(-0.927677032072904,1.00270847417346,1.02927342027029));
#2977=CARTESIAN_POINT('Ctrl Pts',(-0.922321788946925,1.00763658328123,1.02875803347421));
#2978=CARTESIAN_POINT('Ctrl Pts',(-0.91170432487129,1.01725162781242,1.02774996021258));
#2979=CARTESIAN_POINT('Ctrl Pts',(-0.906444773601099,1.02194105831177,1.02725711876946));
#2980=CARTESIAN_POINT('Ctrl Pts',(-0.892866218962798,1.03386042785621,1.02600065843099));
#2981=CARTESIAN_POINT('Ctrl Pts',(-0.884495350603236,1.04103096191356,1.02524114680688));
#2982=CARTESIAN_POINT('Ctrl Pts',(-0.846162385274117,1.07307099156654,1.02182578918361));
#2983=CARTESIAN_POINT('Ctrl Pts',(-0.815229419698272,1.09675600028045,1.01924041416139));
#2984=CARTESIAN_POINT('Ctrl Pts',(-0.700672728752013,1.17694174373649,1.01009118010413));
#2985=CARTESIAN_POINT('Ctrl Pts',(-0.611866859053799,1.22546088975011,1.00374688719229));
#2986=CARTESIAN_POINT('Ctrl Pts',(-0.480888515164538,1.27920179085412,0.994464353421084));
#2987=CARTESIAN_POINT('Ctrl Pts',(-0.442583914750704,1.29295397847068,0.991761330429912));
#2988=CARTESIAN_POINT('Ctrl Pts',(-0.387767925705394,1.30991261058457,0.987872438347571));
#2989=CARTESIAN_POINT('Ctrl Pts',(-0.371721903840006,1.31455612165221,0.986731743680233));
#2990=CARTESIAN_POINT('Ctrl Pts',(-0.343899394152305,1.32205746687706,0.984747683184836));
#2991=CARTESIAN_POINT('Ctrl Pts',(-0.332162359061671,1.32505505163825,0.983908828809258));
#2992=CARTESIAN_POINT('Ctrl Pts',(-0.307928085993631,1.33090216141196,0.982172160868193));
#2993=CARTESIAN_POINT('Ctrl Pts',(-0.295427540803823,1.33373266351745,0.98127384124049));
#2994=CARTESIAN_POINT('Ctrl Pts',(-0.262901436295729,1.3406178631847,0.9789290485056));
#2995=CARTESIAN_POINT('Ctrl Pts',(-0.242822091407495,1.34439978147679,0.977474284569879));
#2996=CARTESIAN_POINT('Ctrl Pts',(-0.139554868590767,1.36146117003613,0.969951361165812));
#2997=CARTESIAN_POINT('Ctrl Pts',(-0.0553648351471,1.36747302604255,0.963665894653975));
#2998=CARTESIAN_POINT('Ctrl Pts',(0.111119535220584,1.36395865656298,0.951084274612596));
#2999=CARTESIAN_POINT('Ctrl Pts',(0.19309051307315,1.3547873754692,0.944819709072733));
#3000=CARTESIAN_POINT('Ctrl Pts',(0.28748088634379,1.335480213202,0.93780658799867));
#3001=CARTESIAN_POINT('Ctrl Pts',(0.301176559409139,1.33245839655782,0.936794395007166));
#3002=CARTESIAN_POINT('Ctrl Pts',(0.322375046547035,1.32743758704017,0.935238503318165));
#3003=CARTESIAN_POINT('Ctrl Pts',(0.329911033883498,1.325584752239,0.934687527724469));
#3004=CARTESIAN_POINT('Ctrl Pts',(0.344027808549043,1.32198608618546,0.933659947133613));
#3005=CARTESIAN_POINT('Ctrl Pts',(0.350611650371849,1.32025520939486,0.933182624483118));
#3006=CARTESIAN_POINT('Ctrl Pts',(0.366536391978728,1.31594110289744,0.932032323226874));
#3007=CARTESIAN_POINT('Ctrl Pts',(0.375863215836806,1.31330756857618,0.931362112621733));
#3008=CARTESIAN_POINT('Ctrl Pts',(0.4101698316904,1.30322528353338,0.928907133783455));
#3009=CARTESIAN_POINT('Ctrl Pts',(0.434964551314517,1.2951607918785,0.92715293432231));
#3010=CARTESIAN_POINT('Ctrl Pts',(0.501703594658899,1.27132076434657,0.922447988664138));
#3011=CARTESIAN_POINT('Ctrl Pts',(0.543128078391972,1.25418316138734,0.919545531620396));
#3012=CARTESIAN_POINT('Ctrl Pts',(0.67692349798588,1.19095598905223,0.910010148093891));
#3013=CARTESIAN_POINT('Ctrl Pts',(0.76490498143937,1.13645048756277,0.903448197219732));
#3014=CARTESIAN_POINT('Ctrl Pts',(0.862453880801481,1.0595155759424,0.895098778056297));
#3015=CARTESIAN_POINT('Ctrl Pts',(0.878692987030042,1.04608723720592,0.893669750023547));
#3016=CARTESIAN_POINT('Ctrl Pts',(0.904398027030114,1.02381044135106,0.891338862302064));
#3017=CARTESIAN_POINT('Ctrl Pts',(0.914060371333503,1.01519319783945,0.890446285170131));
#3018=CARTESIAN_POINT('Ctrl Pts',(0.932482945346784,0.998287014819886,0.888711387356815));
#3019=CARTESIAN_POINT('Ctrl Pts',(0.941258783908613,0.99001681431853,0.887869894260922));
#3020=CARTESIAN_POINT('Ctrl Pts',(0.961670079256935,0.970264830753224,0.88587606079604));
#3021=CARTESIAN_POINT('Ctrl Pts',(0.973210967858884,0.958688455154802,0.884719748248485));
#3022=CARTESIAN_POINT('Ctrl Pts',(1.01298478530772,0.917333917895172,0.880629327979428));
#3023=CARTESIAN_POINT('Ctrl Pts',(1.0400788234312,0.886495982379196,0.877649380150823));
#3024=CARTESIAN_POINT('Ctrl Pts',(1.10901688399886,0.800514488758387,0.869520985454619));
#3025=CARTESIAN_POINT('Ctrl Pts',(1.14812564786238,0.743335590055816,0.864294449373019));
#3026=CARTESIAN_POINT('Ctrl Pts',(1.21703628858013,0.624082920059139,0.853876519721248));
#3027=CARTESIAN_POINT('Ctrl Pts',(1.24682541577135,0.562214445751434,0.848700692153322));
#3028=CARTESIAN_POINT('Ctrl Pts',(1.27634768520716,0.48687261286958,0.842834304629746));
#3029=CARTESIAN_POINT('Ctrl Pts',(1.28069515075193,0.475319169373216,0.841946491388744));
#3030=CARTESIAN_POINT('Ctrl Pts',(1.28737252223326,0.456816877620064,0.840545078818139));
#3031=CARTESIAN_POINT('Ctrl Pts',(1.28980404402359,0.44990577361557,0.840026096186995));
#3032=CARTESIAN_POINT('Ctrl Pts',(1.29445323251035,0.436343868811065,0.839016875223297));
#3033=CARTESIAN_POINT('Ctrl Pts',(1.29667550116893,0.42969499775443,0.838526417961329));
#3034=CARTESIAN_POINT('Ctrl Pts',(1.30220466697686,0.412718538258572,0.837284440516891));
#3035=CARTESIAN_POINT('Ctrl Pts',(1.30544004559378,0.402367857395817,0.836536841081613));
#3036=CARTESIAN_POINT('Ctrl Pts',(1.31911346517483,0.356721625139771,0.833277645772659));
#3037=CARTESIAN_POINT('Ctrl Pts',(1.32824671708704,0.321048011076773,0.830828823665884));
#3038=CARTESIAN_POINT('Ctrl Pts',(1.35407831099748,0.199982698284748,0.822712975968081));
#3039=CARTESIAN_POINT('Ctrl Pts',(1.36406300638835,0.11337803042746,0.817216025408476));
#3040=CARTESIAN_POINT('Ctrl Pts',(1.36678616203293,-0.0274510004467692,
0.808069656315618));
#3041=CARTESIAN_POINT('Ctrl Pts',(1.36464064212542,-0.0813199155979687,
0.804524732361915));
#3042=CARTESIAN_POINT('Ctrl Pts',(1.35753562277348,-0.152904362041534,0.799663494086752));
#3043=CARTESIAN_POINT('Ctrl Pts',(1.35539361442374,-0.170853182351565,0.798432114295665));
#3044=CARTESIAN_POINT('Ctrl Pts',(1.35135963039426,-0.19976687381323,0.796425554654793));
#3045=CARTESIAN_POINT('Ctrl Pts',(1.34968868660415,-0.210760743950194,0.795657218396887));
#3046=CARTESIAN_POINT('Ctrl Pts',(1.34589805872927,-0.233803467809813,0.794034844583878));
#3047=CARTESIAN_POINT('Ctrl Pts',(1.343750369976,-0.245846643418606,0.7931800041941));
#3048=CARTESIAN_POINT('Ctrl Pts',(1.33815415633044,-0.274959420758521,0.791095961382389));
#3049=CARTESIAN_POINT('Ctrl Pts',(1.33454047932909,-0.291994672089594,0.789861736309058));
#3050=CARTESIAN_POINT('Ctrl Pts',(1.31923218988621,-0.357924050461646,0.785025141429504));
#3051=CARTESIAN_POINT('Ctrl Pts',(1.30516895363054,-0.406221764754839,0.781350968541966));
#3052=CARTESIAN_POINT('Ctrl Pts',(1.25157826387111,-0.558439297196694,0.769355688179964));
#3053=CARTESIAN_POINT('Ctrl Pts',(1.20203196062032,-0.658346151971301,0.760802120996546));
#3054=CARTESIAN_POINT('Ctrl Pts',(1.12923931012127,-0.768912910158518,0.751044261213925));
#3055=CARTESIAN_POINT('Ctrl Pts',(1.1171280984892,-0.786405375095243,0.749492398271245));
#3056=CARTESIAN_POINT('Ctrl Pts',(1.09967367435903,-0.810397611144833,0.747359770340762));
#3057=CARTESIAN_POINT('Ctrl Pts',(1.09467223495471,-0.817140860146732,0.746759910639003));
#3058=CARTESIAN_POINT('Ctrl Pts',(1.08551612640903,-0.82925073967982,0.74568242203702));
#3059=CARTESIAN_POINT('Ctrl Pts',(1.08138304307442,-0.83463331619384,0.745203432084687));
#3060=CARTESIAN_POINT('Ctrl Pts',(1.07254061708044,-0.845972978155569,0.744194475430444));
#3061=CARTESIAN_POINT('Ctrl Pts',(1.06782146025793,-0.851921939566133,0.743665180564802));
#3062=CARTESIAN_POINT('Ctrl Pts',(1.05450343250258,-0.868426075851183,0.742195830475928));
#3063=CARTESIAN_POINT('Ctrl Pts',(1.04579575170206,-0.878892837248058,0.74126290075392));
#3064=CARTESIAN_POINT('Ctrl Pts',(1.02548302493403,-0.90257959205657,0.739144467780926));
#3065=CARTESIAN_POINT('Ctrl Pts',(1.01377605236927,-0.915709304396001,0.737964914314965));
#3066=CARTESIAN_POINT('Ctrl Pts',(0.972390391295399,-0.960357665738139,
0.733920175961271));
#3067=CARTESIAN_POINT('Ctrl Pts',(0.941468045953489,-0.990690835827146,
0.73111194018989));
#3068=CARTESIAN_POINT('Ctrl Pts',(0.829839899372953,-1.09023644360328,0.72146843002732));
#3069=CARTESIAN_POINT('Ctrl Pts',(0.742550098032493,-1.15146292774452,0.714720626862009));
#3070=CARTESIAN_POINT('Ctrl Pts',(0.630873626567376,-1.21176778993492,0.70618497768149));
#3071=CARTESIAN_POINT('Ctrl Pts',(0.612477987412635,-1.22116884572154,0.704783182704664));
#3072=CARTESIAN_POINT('Ctrl Pts',(0.582293821502172,-1.23574080897006,0.702485523879612));
#3073=CARTESIAN_POINT('Ctrl Pts',(0.570632552690334,-1.24116876851978,0.701598446494986));
#3074=CARTESIAN_POINT('Ctrl Pts',(0.547862747484823,-1.25137869445491,0.699866518767907));
#3075=CARTESIAN_POINT('Ctrl Pts',(0.536763900918507,-1.2561794159826,0.699022395625653));
#3076=CARTESIAN_POINT('Ctrl Pts',(0.510308137269681,-1.26720803109582,0.697009733439444));
#3077=CARTESIAN_POINT('Ctrl Pts',(0.494899058674679,-1.27330493909369,0.695837004425059));
#3078=CARTESIAN_POINT('Ctrl Pts',(0.439314291503018,-1.29413677860556,0.691603021444579));
#3079=CARTESIAN_POINT('Ctrl Pts',(0.398565778452222,-1.30726113894922,0.688491433962572));
#3080=CARTESIAN_POINT('Ctrl Pts',(0.289746939849012,-1.33674873893412,0.68016247323671));
#3081=CARTESIAN_POINT('Ctrl Pts',(0.220920758644372,-1.34983071270429,0.67487020869525));
#3082=CARTESIAN_POINT('Ctrl Pts',(0.0911551707190771,-1.36430260085462,
0.664996340255401));
#3083=CARTESIAN_POINT('Ctrl Pts',(0.0305221387698023,-1.36700422630184,
0.660426642802755));
#3084=CARTESIAN_POINT('Ctrl Pts',(-0.0450138014688476,-1.36533968399014,
0.654916976798727));
#3085=CARTESIAN_POINT('Ctrl Pts',(-0.0599275413553788,-1.36476643812124,
0.653838249591838));
#3086=CARTESIAN_POINT('Ctrl Pts',(-0.0827695306686175,-1.36351326963545,
0.652202873967985));
#3087=CARTESIAN_POINT('Ctrl Pts',(-0.0907057251456946,-1.36300833128363,
0.651637798445057));
#3088=CARTESIAN_POINT('Ctrl Pts',(-0.104705713736729,-1.36199476213979,
0.650646988521089));
#3089=CARTESIAN_POINT('Ctrl Pts',(-0.110770928450203,-1.36151489973399,
0.650219784784554));
#3090=CARTESIAN_POINT('Ctrl Pts',(-0.125698029025745,-1.36023349889597,
0.649173204512182));
#3091=CARTESIAN_POINT('Ctrl Pts',(-0.134555611766342,-1.35938587760195,
0.648556301204183));
#3092=CARTESIAN_POINT('Ctrl Pts',(-0.163913406787781,-1.35628673010197,
0.646523437734934));
#3093=CARTESIAN_POINT('Ctrl Pts',(-0.184371915954379,-1.35365741820773,
0.645125941602153));
#3094=CARTESIAN_POINT('Ctrl Pts',(-0.334996255337121,-1.33082069734599,
0.634926851666106));
#3095=CARTESIAN_POINT('Ctrl Pts',(-0.461697235191861,-1.29234264611732,
0.626782148790904));
#3096=CARTESIAN_POINT('Ctrl Pts',(-0.612739443756689,-1.2213684941944,0.61578020457222));
#3097=CARTESIAN_POINT('Ctrl Pts',(-0.643950003674871,-1.20520483561193,
0.613434460149172));
#3098=CARTESIAN_POINT('Ctrl Pts',(-0.688145489969292,-1.18010931141388,
0.609982982474489));
#3099=CARTESIAN_POINT('Ctrl Pts',(-0.701655046375404,-1.17212728152373,
0.608909738571869));
#3100=CARTESIAN_POINT('Ctrl Pts',(-0.725255196663827,-1.1576290820534,0.607000578995664));
#3101=CARTESIAN_POINT('Ctrl Pts',(-0.735403113850195,-1.15120911917018,
0.606168161232628));
#3102=CARTESIAN_POINT('Ctrl Pts',(-0.756451654380441,-1.13750112231342,
0.604416581750326));
#3103=CARTESIAN_POINT('Ctrl Pts',(-0.767334567805011,-1.13018828012402,
0.603496573564412));
#3104=CARTESIAN_POINT('Ctrl Pts',(-0.796084768345773,-1.11026272285886,
0.601026449071966));
#3105=CARTESIAN_POINT('Ctrl Pts',(-0.81375660398966,-1.09737612700514,0.599466307248487));
#3106=CARTESIAN_POINT('Ctrl Pts',(-0.884762041809014,-1.04293933680528,
0.593019895953218));
#3107=CARTESIAN_POINT('Ctrl Pts',(-0.935278502704825,-0.997886834144783,
0.5880043158672));
#3108=CARTESIAN_POINT('Ctrl Pts',(-1.03526868624114,-0.894424880740563,
0.577172516095617));
#3109=CARTESIAN_POINT('Ctrl Pts',(-1.08360069506678,-0.83521675611104,0.571353707097514));
#3110=CARTESIAN_POINT('Ctrl Pts',(-1.14233896367567,-0.749519353743777,
0.563639454464373));
#3111=CARTESIAN_POINT('Ctrl Pts',(-1.1572488417153,-0.726287082800166,0.561613254277114));
#3112=CARTESIAN_POINT('Ctrl Pts',(-1.17666668426288,-0.693912492256261,
0.558892387332601));
#3113=CARTESIAN_POINT('Ctrl Pts',(-1.18179072441828,-0.685149423308594,
0.558165888912684));
#3114=CARTESIAN_POINT('Ctrl Pts',(-1.19018966968345,-0.670411036053599,
0.556961579801388));
#3115=CARTESIAN_POINT('Ctrl Pts',(-1.19351834800689,-0.664466980674374,
0.556480591483509));
#3116=CARTESIAN_POINT('Ctrl Pts',(-1.2004296492375,-0.651905873887536,0.555474363452153));
#3117=CARTESIAN_POINT('Ctrl Pts',(-1.20400229361304,-0.64528373219101,0.554949716038826));
#3118=CARTESIAN_POINT('Ctrl Pts',(-1.21373972330462,-0.626872286024494,
0.553506160624112));
#3119=CARTESIAN_POINT('Ctrl Pts',(-1.21978746794125,-0.615021580990691,
0.552593994222108));
#3120=CARTESIAN_POINT('Ctrl Pts',(-1.25669945158538,-0.540004496585257,
0.546913876345834));
#3121=CARTESIAN_POINT('Ctrl Pts',(-1.28282565801612,-0.47461478826364,0.54237433823007));
#3122=CARTESIAN_POINT('Ctrl Pts',(-1.33189446435503,-0.317617117155719,
0.531792766946884));
#3123=CARTESIAN_POINT('Ctrl Pts',(-1.35061430885415,-0.225082976948201,
0.525778325928075));
#3124=CARTESIAN_POINT('Ctrl Pts',(-1.36177845043777,-0.109529145641503,
0.517993482619221));
#3125=CARTESIAN_POINT('Ctrl Pts',(-1.3633616009835,-0.0876483812206271,
0.516508640083566));
#3126=CARTESIAN_POINT('Ctrl Pts',(-1.36502239500673,-0.0531789904680141,
0.514147489695694));
#3127=CARTESIAN_POINT('Ctrl Pts',(-1.36545410072905,-0.0406106475250119,
0.513281978098375));
#3128=CARTESIAN_POINT('Ctrl Pts',(-1.36590527229224,-0.0186347628800302,
0.511759778070425));
#3129=CARTESIAN_POINT('Ctrl Pts',(-1.36600119826705,-0.00922954513205333,
0.51110548077593));
#3130=CARTESIAN_POINT('Ctrl Pts',(-1.3659999887036,0.000175675168235992,
0.510448192708096));
#3131=CARTESIAN_POINT('Ctrl Pts',(-1.14737960344596,0.741266514552077,0.454399650883576));
#3132=CARTESIAN_POINT('Ctrl Pts',(-1.16980381270752,0.706556892810074,0.457297104121828));
#3133=CARTESIAN_POINT('Ctrl Pts',(-1.19062132235074,0.67087574888106,0.460194557360079));
#3134=CARTESIAN_POINT('Ctrl Pts',(-1.209754948191,0.634388654790895,0.46309201059833));
#3135=CARTESIAN_POINT('Ctrl Pts',(-1.23535670833523,0.585567075490906,0.466968949734391));
#3136=CARTESIAN_POINT('Ctrl Pts',(-1.25804035543911,0.535115314397402,0.470845888870453));
#3137=CARTESIAN_POINT('Ctrl Pts',(-1.27760921812476,0.4833949583546,0.474722828006513));
#3138=CARTESIAN_POINT('Ctrl Pts',(-1.2971361549215,0.431785412118988,0.478591460879605));
#3139=CARTESIAN_POINT('Ctrl Pts',(-1.31356140704316,0.378913085531293,0.482460093752696));
#3140=CARTESIAN_POINT('Ctrl Pts',(-1.32673491272539,0.325162223137256,0.486328726625788));
#3141=CARTESIAN_POINT('Ctrl Pts',(-1.33987073668409,0.271565110639755,0.490186293594493));
#3142=CARTESIAN_POINT('Ctrl Pts',(-1.34977321737813,0.217094895152634,0.494043860563197));
#3143=CARTESIAN_POINT('Ctrl Pts',(-1.35634174144863,0.162151411970686,0.497901427531902));
#3144=CARTESIAN_POINT('Ctrl Pts',(-1.36276129738084,0.108453996902938,0.501671508398166));
#3145=CARTESIAN_POINT('Ctrl Pts',(-1.36599645439874,0.0543049796234106,
0.505441589264431));
#3146=CARTESIAN_POINT('Ctrl Pts',(-1.36599999708368,8.92602306106192E-5,
0.509211670130695));
#3147=CARTESIAN_POINT('',(-1.36714090672731,0.00103847535578433,0.390789005901724));
#3148=CARTESIAN_POINT('Ctrl Pts',(-1.14737960344596,0.741266514552078,0.335993717254284));
#3149=CARTESIAN_POINT('Ctrl Pts',(-1.17597380908877,0.697006578770251,0.339667702888683));
#3150=CARTESIAN_POINT('Ctrl Pts',(-1.20199560468014,0.65110181371439,0.343341688523083));
#3151=CARTESIAN_POINT('Ctrl Pts',(-1.22526698137143,0.603884777387997,0.347015674157483));
#3152=CARTESIAN_POINT('Ctrl Pts',(-1.24854868955544,0.556646778723448,0.350691290883863));
#3153=CARTESIAN_POINT('Ctrl Pts',(-1.2690773348328,0.508095840000956,0.354366907610241));
#3154=CARTESIAN_POINT('Ctrl Pts',(-1.28672281254762,0.458585219637033,0.358042524336621));
#3155=CARTESIAN_POINT('Ctrl Pts',(-1.30440173491501,0.408980758487189,0.361725107704901));
#3156=CARTESIAN_POINT('Ctrl Pts',(-1.31918642143983,0.358413495999061,0.365407691073181));
#3157=CARTESIAN_POINT('Ctrl Pts',(-1.33099684162401,0.307251375240078,0.36909027444146));
#3158=CARTESIAN_POINT('Ctrl Pts',(-1.34002691658575,0.268133564150332,0.371905923956875));
#3159=CARTESIAN_POINT('Ctrl Pts',(-1.34731930023076,0.228668325964515,0.374721573472289));
#3160=CARTESIAN_POINT('Ctrl Pts',(-1.35285868001946,0.189022199479346,0.377537222987704));
#3161=CARTESIAN_POINT('Ctrl Pts',(-1.36154855341204,0.126827543614587,0.381954258601826));
#3162=CARTESIAN_POINT('Ctrl Pts',(-1.36595132362477,0.0640157464585561,
0.386371294215948));
#3163=CARTESIAN_POINT('Ctrl Pts',(-1.36599959856312,0.00104724658421214,
0.390788329830071));
#3164=CARTESIAN_POINT('Ctrl Pts',(-1.36716844264157,0.00103826373564391,
0.390789022213051));
#3165=CARTESIAN_POINT('Ctrl Pts',(-1.36407996739449,-0.384831305017282,
0.417833191053577));
#3166=CARTESIAN_POINT('Ctrl Pts',(-0.993135927374991,-1.22506008325323,
0.476338795143076));
#3167=CARTESIAN_POINT('Ctrl Pts',(0.425019159697173,-1.55235943515438,0.566305834481554));
#3168=CARTESIAN_POINT('Ctrl Pts',(1.53026813668533,-0.498999262857103,0.660690140228478));
#3169=CARTESIAN_POINT('Ctrl Pts',(1.25840837427535,1.00357516935923,0.755074445975404));
#3170=CARTESIAN_POINT('Ctrl Pts',(-0.10689282456352,1.58625723301147,0.84683417891952));
#3171=CARTESIAN_POINT('Ctrl Pts',(-0.923664677800894,1.08605463080936,0.90713247661466));
#3172=CARTESIAN_POINT('Ctrl Pts',(-1.14885860607148,0.742234466194312,0.935969339060826));
#3173=CARTESIAN_POINT('Origin',(0.,0.,-1.10921167016993));
#3174=CARTESIAN_POINT('',(-1.14737959979828,0.741266520198191,1.65532966579394));
#3175=CARTESIAN_POINT('',(-1.14737969890459,0.741266366795107,1.5357812853031));
#3176=CARTESIAN_POINT('',(-1.14737960344596,0.741266514552077,-1.10921167016993));
#3177=CARTESIAN_POINT('Ctrl Pts',(-1.14737959979828,0.741266520198191,1.65532966579394));
#3178=CARTESIAN_POINT('Ctrl Pts',(-1.13157732704963,0.765726285867094,1.65340285213149));
#3179=CARTESIAN_POINT('Ctrl Pts',(-1.11499628676279,0.789675525276667,1.65145455257775));
#3180=CARTESIAN_POINT('Ctrl Pts',(-1.09618984841233,0.815064371089371,1.64931104945167));
#3181=CARTESIAN_POINT('Ctrl Pts',(-1.09471282790514,0.817047083754974,1.64914312583003));
#3182=CARTESIAN_POINT('Ctrl Pts',(-1.09203671576753,0.820619141406182,1.64883962896734));
#3183=CARTESIAN_POINT('Ctrl Pts',(-1.09083951413336,0.822209899091305,1.64870412408433));
#3184=CARTESIAN_POINT('Ctrl Pts',(-1.08863657816546,0.825123725688757,1.64845527392725));
#3185=CARTESIAN_POINT('Ctrl Pts',(-1.08763189726973,0.826447589394383,1.64834196717432));
#3186=CARTESIAN_POINT('Ctrl Pts',(-1.08575151311276,0.82891599611319,1.64813024171768));
#3187=CARTESIAN_POINT('Ctrl Pts',(-1.08487640885809,0.830060994334693,1.64803184511967));
#3188=CARTESIAN_POINT('Ctrl Pts',(-1.08320819288929,0.832236566109536,1.64784453049659));
#3189=CARTESIAN_POINT('Ctrl Pts',(-1.0824154177483,0.833267396766278,1.64775562499771));
#3190=CARTESIAN_POINT('Ctrl Pts',(-1.08087361045307,0.835266266755387,1.64758293302855));
#3191=CARTESIAN_POINT('Ctrl Pts',(-1.08012474656809,0.836234434825733,1.64749915288156));
#3192=CARTESIAN_POINT('Ctrl Pts',(-1.07136207112076,0.847531844260759,1.64651994512447));
#3193=CARTESIAN_POINT('Ctrl Pts',(-1.06320191857769,0.857746218013062,1.64561905816151));
#3194=CARTESIAN_POINT('Ctrl Pts',(-1.04726522499238,0.877117915237756,1.6438793225995));
#3195=CARTESIAN_POINT('Ctrl Pts',(-1.03951199119753,0.886292893270802,1.64304145020067));
#3196=CARTESIAN_POINT('Ctrl Pts',(-1.02131423617514,0.907260354219105,1.64109348573989));
#3197=CARTESIAN_POINT('Ctrl Pts',(-1.01078489732438,0.918976590491354,1.63998001589182));
#3198=CARTESIAN_POINT('Ctrl Pts',(-0.975800267832639,0.956576040269497,
1.6363223781997));
#3199=CARTESIAN_POINT('Ctrl Pts',(-0.950536957374356,0.981683744160941,
1.63374519266463));
#3200=CARTESIAN_POINT('Ctrl Pts',(-0.827648614567908,1.09462024340742,1.62149315287158));
#3201=CARTESIAN_POINT('Ctrl Pts',(-0.718687769668506,1.16904921015942,1.61133802036522));
#3202=CARTESIAN_POINT('Ctrl Pts',(-0.582325191167811,1.23583021295908,1.60016533406788));
#3203=CARTESIAN_POINT('Ctrl Pts',(-0.563652377964652,1.24445773362186,1.59866763668675));
#3204=CARTESIAN_POINT('Ctrl Pts',(-0.536643199072388,1.25620420874822,1.59655382827057));
#3205=CARTESIAN_POINT('Ctrl Pts',(-0.528461052119848,1.25966815650352,1.59592025298032));
#3206=CARTESIAN_POINT('Ctrl Pts',(-0.514623531442021,1.2653677680976,1.59486081727722));
#3207=CARTESIAN_POINT('Ctrl Pts',(-0.508986191775682,1.26764586126778,1.59443257253152));
#3208=CARTESIAN_POINT('Ctrl Pts',(-0.495939338273296,1.27281712568727,1.59344929703094));
#3209=CARTESIAN_POINT('Ctrl Pts',(-0.488519503045984,1.27568333289407,1.592895817731));
#3210=CARTESIAN_POINT('Ctrl Pts',(-0.467095814635799,1.28374474923591,1.59131295322562));
#3211=CARTESIAN_POINT('Ctrl Pts',(-0.453030761263395,1.28877548701948,1.59029236419117));
#3212=CARTESIAN_POINT('Ctrl Pts',(-0.381314162641116,1.31310756518761,1.58516857237657));
#3213=CARTESIAN_POINT('Ctrl Pts',(-0.322496554436863,1.32877747540901,1.58122482071883));
#3214=CARTESIAN_POINT('Ctrl Pts',(-0.209358126060383,1.35096030710697,1.5737964073502));
#3215=CARTESIAN_POINT('Ctrl Pts',(-0.155313087492419,1.35823499743524,1.57031321191162));
#3216=CARTESIAN_POINT('Ctrl Pts',(-0.0640505476519799,1.3649998892132,1.5643728572327));
#3217=CARTESIAN_POINT('Ctrl Pts',(-0.0270287085696955,1.36623436238396,
1.5619475656185));
#3218=CARTESIAN_POINT('Ctrl Pts',(0.0375925412209382,1.36576148153045,1.55764651497081));
#3219=CARTESIAN_POINT('Ctrl Pts',(0.0651752125591951,1.36472328603271,1.55578924772369));
#3220=CARTESIAN_POINT('Ctrl Pts',(0.106897417192534,1.36188518906193,1.55293672271717));
#3221=CARTESIAN_POINT('Ctrl Pts',(0.121072339273535,1.36069827252482,1.55196004321749));
#3222=CARTESIAN_POINT('Ctrl Pts',(0.147030469113191,1.35811589078796,1.55015629090638));
#3223=CARTESIAN_POINT('Ctrl Pts',(0.158819099150086,1.3567878278786,1.54933136815925));
#3224=CARTESIAN_POINT('Ctrl Pts',(0.184753951117711,1.35352348080542,1.54750309522908));
#3225=CARTESIAN_POINT('Ctrl Pts',(0.198889962799352,1.3515186239245,1.5464977174662));
#3226=CARTESIAN_POINT('Ctrl Pts',(0.239671234317948,1.34508112949963,1.54357039161257));
#3227=CARTESIAN_POINT('Ctrl Pts',(0.266218411995413,1.34007952061447,1.54163130482753));
#3228=CARTESIAN_POINT('Ctrl Pts',(0.391271416578256,1.31265656760955,1.53233212369918));
#3229=CARTESIAN_POINT('Ctrl Pts',(0.487227415380485,1.28014221812151,1.52467441351063));
#3230=CARTESIAN_POINT('Ctrl Pts',(0.613975549195938,1.2208628589983,1.51410791260819));
#3231=CARTESIAN_POINT('Ctrl Pts',(0.648526424390272,1.20286571048635,1.51118118289506));
#3232=CARTESIAN_POINT('Ctrl Pts',(0.70293794930403,1.17149638267966,1.50653954856131));
#3233=CARTESIAN_POINT('Ctrl Pts',(0.72329864407153,1.1590361388582,1.50479504611658));
#3234=CARTESIAN_POINT('Ctrl Pts',(0.751200485149323,1.14093907548456,1.50240394369346));
#3235=CARTESIAN_POINT('Ctrl Pts',(0.759024618434151,1.13574899700753,1.50173339362481));
#3236=CARTESIAN_POINT('Ctrl Pts',(0.772394788113732,1.12668011327739,1.50058827360131));
#3237=CARTESIAN_POINT('Ctrl Pts',(0.777966496633989,1.12284011522064,1.50011132569043));
#3238=CARTESIAN_POINT('Ctrl Pts',(0.789998762271181,1.11441496178589,1.49908207692748));
#3239=CARTESIAN_POINT('Ctrl Pts',(0.796448281383773,1.10981480185904,1.49853075880253));
#3240=CARTESIAN_POINT('Ctrl Pts',(0.814817394342888,1.09647030849328,1.49696046975757));
#3241=CARTESIAN_POINT('Ctrl Pts',(0.826635953658063,1.08758795861832,1.49595008233042));
#3242=CARTESIAN_POINT('Ctrl Pts',(0.883949331738296,1.04303939534848,1.49103713249067));
#3243=CARTESIAN_POINT('Ctrl Pts',(0.927297354056396,1.00469829895977,1.48727847335196));
#3244=CARTESIAN_POINT('Ctrl Pts',(1.01998784567374,0.911587744246213,1.47880513393602));
#3245=CARTESIAN_POINT('Ctrl Pts',(1.06758868727028,0.855348711828194,1.47411867390129));
#3246=CARTESIAN_POINT('Ctrl Pts',(1.13511255015301,0.761099030570097,1.46652308406284));
#3247=CARTESIAN_POINT('Ctrl Pts',(1.15817676408061,0.725519322274498,1.4637084902383));
#3248=CARTESIAN_POINT('Ctrl Pts',(1.18787990540595,0.674663042408695,1.45971519310126));
#3249=CARTESIAN_POINT('Ctrl Pts',(1.19595152740628,0.660249040149263,1.45858668759304));
#3250=CARTESIAN_POINT('Ctrl Pts',(1.20947166205826,0.635043566939719,1.45661680995541));
#3251=CARTESIAN_POINT('Ctrl Pts',(1.21504210182008,0.624319395639666,1.45577976885854));
#3252=CARTESIAN_POINT('Ctrl Pts',(1.22625459015882,0.602014611412802,1.45404027590548));
#3253=CARTESIAN_POINT('Ctrl Pts',(1.23187655440053,0.590425310145571,1.45313723932975));
#3254=CARTESIAN_POINT('Ctrl Pts',(1.24612414164939,0.559965254266523,1.45076491473821));
#3255=CARTESIAN_POINT('Ctrl Pts',(1.25448489957484,0.540975060079367,1.44928696295526));
#3256=CARTESIAN_POINT('Ctrl Pts',(1.30274543076363,0.42421722483658,1.4402013830026));
#3257=CARTESIAN_POINT('Ctrl Pts',(1.33162344036849,0.322299666113666,1.43223568499318));
#3258=CARTESIAN_POINT('Ctrl Pts',(1.35543875472185,0.175051978015087,1.42095794797091));
#3259=CARTESIAN_POINT('Ctrl Pts',(1.36033606789949,0.1316951096914,1.41767056900508));
#3260=CARTESIAN_POINT('Ctrl Pts',(1.36480587007387,0.0625946555582757,1.41254245531937));
#3261=CARTESIAN_POINT('Ctrl Pts',(1.3657403127223,0.0369695940772661,1.41066509672106));
#3262=CARTESIAN_POINT('Ctrl Pts',(1.36603291079038,0.00169869731663778,
1.40812702760474));
#3263=CARTESIAN_POINT('Ctrl Pts',(1.36601092469451,-0.00793512638533304,
1.40743850892886));
#3264=CARTESIAN_POINT('Ctrl Pts',(1.3657995827943,-0.0243664154470303,1.40627311981112));
#3265=CARTESIAN_POINT('Ctrl Pts',(1.36566139112101,-0.0311640127470081,
1.40579363266095));
#3266=CARTESIAN_POINT('Ctrl Pts',(1.36525601021453,-0.0457458357883727,
1.4047709463584));
#3267=CARTESIAN_POINT('Ctrl Pts',(1.36497299857079,-0.0535292035892514,
1.40422858085078));
#3268=CARTESIAN_POINT('Ctrl Pts',(1.36398811968669,-0.0754504161648913,
1.40270988709086));
#3269=CARTESIAN_POINT('Ctrl Pts',(1.36313303449358,-0.089580831262057,1.40174129523892));
#3270=CARTESIAN_POINT('Ctrl Pts',(1.35599886749487,-0.183288830481665,1.39537160295281));
#3271=CARTESIAN_POINT('Ctrl Pts',(1.34297358179724,-0.262207804118862,1.39025853295132));
#3272=CARTESIAN_POINT('Ctrl Pts',(1.30124664725503,-0.42480771320341,1.37946772875809));
#3273=CARTESIAN_POINT('Ctrl Pts',(1.27117918385615,-0.507745485106411,1.37380390350069));
#3274=CARTESIAN_POINT('Ctrl Pts',(1.2248906524783,-0.6049675230205,1.36654940931271));
#3275=CARTESIAN_POINT('Ctrl Pts',(1.21605388867345,-0.622539709065144,1.36521285771542));
#3276=CARTESIAN_POINT('Ctrl Pts',(1.2009086985965,-0.651102658503491,1.3629945352084));
#3277=CARTESIAN_POINT('Ctrl Pts',(1.19482106669932,-0.662207651953928,1.36212039962681));
#3278=CARTESIAN_POINT('Ctrl Pts',(1.18263673340026,-0.68371908208986,1.3604032463307));
#3279=CARTESIAN_POINT('Ctrl Pts',(1.17655485970583,-0.694132604098824,1.35956081092558));
#3280=CARTESIAN_POINT('Ctrl Pts',(1.16289587070979,-0.716824478669667,1.35769966294096));
#3281=CARTESIAN_POINT('Ctrl Pts',(1.15526057367156,-0.729065921551139,1.35667894141426));
#3282=CARTESIAN_POINT('Ctrl Pts',(1.12812899701686,-0.771068554796105,1.35311693600891));
#3283=CARTESIAN_POINT('Ctrl Pts',(1.10766645147329,-0.800185216770624,1.35054138397971));
#3284=CARTESIAN_POINT('Ctrl Pts',(1.00656548959112,-0.932725039616337,1.33830225576582));
#3285=CARTESIAN_POINT('Ctrl Pts',(0.912457086631124,-1.02497058099155,1.32816074412412));
#3286=CARTESIAN_POINT('Ctrl Pts',(0.790090475053509,-1.11451089361474,1.31700399001067));
#3287=CARTESIAN_POINT('Ctrl Pts',(0.773249869817719,-1.12626028940802,1.31550893075498));
#3288=CARTESIAN_POINT('Ctrl Pts',(0.748755252895523,-1.14254120537556,1.3133981193078));
#3289=CARTESIAN_POINT('Ctrl Pts',(0.741312769643017,-1.14738407832488,1.3127649672859));
#3290=CARTESIAN_POINT('Ctrl Pts',(0.728695630625511,-1.15542011298492,1.31170600298635));
#3291=CARTESIAN_POINT('Ctrl Pts',(0.723546119789299,-1.15865179301619,1.31127781176725));
#3292=CARTESIAN_POINT('Ctrl Pts',(0.71160650986227,-1.1660340902125,1.31029432538927));
#3293=CARTESIAN_POINT('Ctrl Pts',(0.70480147755425,-1.17015990772813,1.30974058578339));
#3294=CARTESIAN_POINT('Ctrl Pts',(0.685105528684215,-1.18186718881086,1.30815619751506));
#3295=CARTESIAN_POINT('Ctrl Pts',(0.672125224610417,-1.18929700469306,1.3071343710307));
#3296=CARTESIAN_POINT('Ctrl Pts',(0.605547051049838,-1.22596747115425,1.3019920417282));
#3297=CARTESIAN_POINT('Ctrl Pts',(0.550148437685273,-1.25180742227082,1.29803234143895));
#3298=CARTESIAN_POINT('Ctrl Pts',(0.441199273615448,-1.29398947432656,1.29050547070303));
#3299=CARTESIAN_POINT('Ctrl Pts',(0.388014332740054,-1.31091963926611,1.28694094239898));
#3300=CARTESIAN_POINT('Ctrl Pts',(0.281838612941561,-1.33768851156519,1.27982747121024));
#3301=CARTESIAN_POINT('Ctrl Pts',(0.229008622398246,-1.34773797395584,1.27628896444022));
#3302=CARTESIAN_POINT('Ctrl Pts',(0.158129251480435,-1.35693259513905,1.27145572110254));
#3303=CARTESIAN_POINT('Ctrl Pts',(0.140488398532634,-1.35887228587463,1.27024607528252));
#3304=CARTESIAN_POINT('Ctrl Pts',(0.11057118219621,-1.36157304499883,1.26818060616542));
#3305=CARTESIAN_POINT('Ctrl Pts',(0.0983129365656097,-1.362513006413,1.26733034208558));
#3306=CARTESIAN_POINT('Ctrl Pts',(0.0735425453086204,-1.36407639201882,
1.26560338430746));
#3307=CARTESIAN_POINT('Ctrl Pts',(0.0610311989708883,-1.36469340275687,
1.26472657895214));
#3308=CARTESIAN_POINT('Ctrl Pts',(0.0295547822926375,-1.36581199350444,
1.26250846074222));
#3309=CARTESIAN_POINT('Ctrl Pts',(0.0105849825755796,-1.36609069275984,
1.26116050162535));
#3310=CARTESIAN_POINT('Ctrl Pts',(-0.0760357699270293,-1.3655590587654,
1.25495115622482));
#3311=CARTESIAN_POINT('Ctrl Pts',(-0.143553530846213,-1.36011871736758,
1.24995341463193));
#3312=CARTESIAN_POINT('Ctrl Pts',(-0.3048634630354,-1.33497487584253,1.23768901239036));
#3313=CARTESIAN_POINT('Ctrl Pts',(-0.397537925459773,-1.31036792905016,
1.23036176982192));
#3314=CARTESIAN_POINT('Ctrl Pts',(-0.503806367226208,-1.26982801047383,
1.22202347632841));
#3315=CARTESIAN_POINT('Ctrl Pts',(-0.520599444622563,-1.26303615480609,
1.22070860304169));
#3316=CARTESIAN_POINT('Ctrl Pts',(-0.545037031249402,-1.25258225503137,
1.21880413648154));
#3317=CARTESIAN_POINT('Ctrl Pts',(-0.552789768928874,-1.24918019195862,
1.2182012994533));
#3318=CARTESIAN_POINT('Ctrl Pts',(-0.566023340487419,-1.2432256917826,1.21717520673911));
#3319=CARTESIAN_POINT('Ctrl Pts',(-0.571519480170527,-1.24070868077049,
1.216749961424));
#3320=CARTESIAN_POINT('Ctrl Pts',(-0.58450832064387,-1.23465568388712,1.21574712916741));
#3321=CARTESIAN_POINT('Ctrl Pts',(-0.591985816169586,-1.23108790792638,
1.21517143350831));
#3322=CARTESIAN_POINT('Ctrl Pts',(-0.614810946185485,-1.21994117487299,
1.21341770018541));
#3323=CARTESIAN_POINT('Ctrl Pts',(-0.630049606176986,-1.21214129939181,
1.21225186849617));
#3324=CARTESIAN_POINT('Ctrl Pts',(-0.720803745453559,-1.16351485954236,
1.20531489930424));
#3325=CARTESIAN_POINT('Ctrl Pts',(-0.792487961997044,-1.11592613945786,
1.19985275676933));
#3326=CARTESIAN_POINT('Ctrl Pts',(-0.899960954706448,-1.02896577508745,
1.19095788458645));
#3327=CARTESIAN_POINT('Ctrl Pts',(-0.938754056362153,-0.993700446105792,
1.18757376884359));
#3328=CARTESIAN_POINT('Ctrl Pts',(-0.99981992989095,-0.931413141811491,
1.18181774950615));
#3329=CARTESIAN_POINT('Ctrl Pts',(-1.02325259697926,-0.90560705522448,1.17948890840282));
#3330=CARTESIAN_POINT('Ctrl Pts',(-1.05561843802805,-0.867101312770434,
1.17606954363348));
#3331=CARTESIAN_POINT('Ctrl Pts',(-1.06536322526795,-0.855100075337538,
1.17501121988319));
#3332=CARTESIAN_POINT('Ctrl Pts',(-1.08227001783854,-0.83354074675601,1.1731212235882));
#3333=CARTESIAN_POINT('Ctrl Pts',(-1.08951439314667,-0.824049112244289,
1.17229286615374));
#3334=CARTESIAN_POINT('Ctrl Pts',(-1.10459476690387,-0.803744176684975,
1.17052786589274));
#3335=CARTESIAN_POINT('Ctrl Pts',(-1.11239844606318,-0.792908554252095,
1.16959010806056));
#3336=CARTESIAN_POINT('Ctrl Pts',(-1.13325946616582,-0.763028258460327,
1.16701427138683));
#3337=CARTESIAN_POINT('Ctrl Pts',(-1.14599423610522,-0.743764907222998,
1.16536458182868));
#3338=CARTESIAN_POINT('Ctrl Pts',(-1.22478611878269,-0.617748863874061,
1.15463541675137));
#3339=CARTESIAN_POINT('Ctrl Pts',(-1.27633928039711,-0.50265420886069,1.14503984477189));
#3340=CARTESIAN_POINT('Ctrl Pts',(-1.32308195813287,-0.342256069747352,
1.13250260758063));
#3341=CARTESIAN_POINT('Ctrl Pts',(-1.33288802714624,-0.301819924240409,
1.12941581173562));
#3342=CARTESIAN_POINT('Ctrl Pts',(-1.3429784543516,-0.249981559509147,1.12559793785485));
#3343=CARTESIAN_POINT('Ctrl Pts',(-1.34498668216468,-0.238940902006796,
1.12479275219632));
#3344=CARTESIAN_POINT('Ctrl Pts',(-1.34804102960402,-0.220888237432621,
1.12349045250493));
#3345=CARTESIAN_POINT('Ctrl Pts',(-1.34916898496192,-0.213890832000283,
1.12298914849105));
#3346=CARTESIAN_POINT('Ctrl Pts',(-1.35133703327292,-0.19974096666365,1.12198287222489));
#3347=CARTESIAN_POINT('Ctrl Pts',(-1.35237492353611,-0.192588430649364,
1.12147802405521));
#3348=CARTESIAN_POINT('Ctrl Pts',(-1.35496873258695,-0.173657356554059,
1.12015106283942));
#3349=CARTESIAN_POINT('Ctrl Pts',(-1.35642788350477,-0.16186588527212,1.11933399261896));
#3350=CARTESIAN_POINT('Ctrl Pts',(-1.36320088912587,-0.100582694163536,
1.11512939661801));
#3351=CARTESIAN_POINT('Ctrl Pts',(-1.3659611275071,-0.0508413741491877,
1.11185760075806));
#3352=CARTESIAN_POINT('Ctrl Pts',(-1.36608560145227,0.110268494496373,1.10140450719495));
#3353=CARTESIAN_POINT('Ctrl Pts',(-1.35256365678427,0.221178661717358,1.0943951332629));
#3354=CARTESIAN_POINT('Ctrl Pts',(-1.32013206461214,0.351777820116467,1.08541682949322));
#3355=CARTESIAN_POINT('Ctrl Pts',(-1.31395532898235,0.374189250266236,1.08385104960099));
#3356=CARTESIAN_POINT('Ctrl Pts',(-1.30295487259447,0.410462652564167,1.08126885063572));
#3357=CARTESIAN_POINT('Ctrl Pts',(-1.29847412286516,0.424424213827309,1.08026319994651));
#3358=CARTESIAN_POINT('Ctrl Pts',(-1.28995975318309,0.449556244798788,1.07843007567478));
#3359=CARTESIAN_POINT('Ctrl Pts',(-1.286003502312,0.460751514999018,1.07760516809675));
#3360=CARTESIAN_POINT('Ctrl Pts',(-1.27710652106028,0.484920226046374,1.07580545425383));
#3361=CARTESIAN_POINT('Ctrl Pts',(-1.27211299595738,0.497872666528782,1.07482899979953));
#3362=CARTESIAN_POINT('Ctrl Pts',(-1.25728339813184,0.53465797163118,1.07202035033582));
#3363=CARTESIAN_POINT('Ctrl Pts',(-1.24696928439987,0.558290368356846,1.07017273559371));
#3364=CARTESIAN_POINT('Ctrl Pts',(-1.2145883724344,0.627103172903603,1.0646605492661));
#3365=CARTESIAN_POINT('Ctrl Pts',(-1.19069091880293,0.671369855409078,1.06094017952552));
#3366=CARTESIAN_POINT('Ctrl Pts',(-1.15883876703743,0.723299585331697,1.05637300530005));
#3367=CARTESIAN_POINT('Ctrl Pts',(-1.15316122838722,0.732317346808646,1.05557222496468));
#3368=CARTESIAN_POINT('Ctrl Pts',(-1.14737959575237,0.741266526460718,1.05477007217181));
#3369=CARTESIAN_POINT('',(-1.36400241667853,1.39474960495158E-5,0.990700274402563));
#3370=CARTESIAN_POINT('Ctrl Pts',(-1.14885860607148,0.742234466194312,0.935969339060826));
#3371=CARTESIAN_POINT('Ctrl Pts',(-1.16935452030627,0.710941843607821,0.938593911863636));
#3372=CARTESIAN_POINT('Ctrl Pts',(-1.30251261166389,0.487041195934633,0.9568669035642));
#3373=CARTESIAN_POINT('Ctrl Pts',(-1.36387713097247,0.224696456629905,0.975139895264764));
#3374=CARTESIAN_POINT('Ctrl Pts',(-1.36384943109475,2.00760032713424E-5,
0.990788314162518));
#3375=CARTESIAN_POINT('Ctrl Pts',(-1.36599999840197,-6.6074383892362E-5,
0.989550711083759));
#3376=CARTESIAN_POINT('Ctrl Pts',(-1.36599971820694,-0.00585873393595662,
0.989953076044015));
#3377=CARTESIAN_POINT('Ctrl Pts',(-1.36596259150209,-0.011651267602572,
0.990356560016656));
#3378=CARTESIAN_POINT('Ctrl Pts',(-1.36578899683438,-0.0252444878524435,
0.991306141617785));
#3379=CARTESIAN_POINT('Ctrl Pts',(-1.36562254090052,-0.0330445056752,0.991853141539721));
#3380=CARTESIAN_POINT('Ctrl Pts',(-1.36490816371014,-0.0569265470916234,
0.993534654597446));
#3381=CARTESIAN_POINT('Ctrl Pts',(-1.3641429041869,-0.0730001705183924,
0.994675728498607));
#3382=CARTESIAN_POINT('Ctrl Pts',(-1.36007357431624,-0.135285506229272,
0.999135492985641));
#3383=CARTESIAN_POINT('Ctrl Pts',(-1.35470372623049,-0.181326384655276,
1.00251504937969));
#3384=CARTESIAN_POINT('Ctrl Pts',(-1.32760515654106,-0.342127015480296,
1.01460520713435));
#3385=CARTESIAN_POINT('Ctrl Pts',(-1.29352781976786,-0.454278660724451,
1.02360662992386));
#3386=CARTESIAN_POINT('Ctrl Pts',(-1.23709430889794,-0.579641219598352,
1.03372539977164));
#3387=CARTESIAN_POINT('Ctrl Pts',(-1.22814924475359,-0.598360943080897,
1.03523634447006));
#3388=CARTESIAN_POINT('Ctrl Pts',(-1.21475642286182,-0.624821770877291,
1.03736503505638));
#3389=CARTESIAN_POINT('Ctrl Pts',(-1.2106543024637,-0.632733421903402,1.03800057467419));
#3390=CARTESIAN_POINT('Ctrl Pts',(-1.20362293793128,-0.645975856424783,
1.03906207707982));
#3391=CARTESIAN_POINT('Ctrl Pts',(-1.20073509571223,-0.651328042645779,
1.03949045058018));
#3392=CARTESIAN_POINT('Ctrl Pts',(-1.1939988674979,-0.663615554845057,1.04047229726013));
#3393=CARTESIAN_POINT('Ctrl Pts',(-1.19012569366639,-0.670536905338416,
1.04102424118296));
#3394=CARTESIAN_POINT('Ctrl Pts',(-1.17883665185755,-0.690304389260967,
1.04259854532155));
#3395=CARTESIAN_POINT('Ctrl Pts',(-1.1712712992169,-0.703064427855035,1.04361225254016));
#3396=CARTESIAN_POINT('Ctrl Pts',(-1.12687739197088,-0.775234784811891,
1.04934623798698));
#3397=CARTESIAN_POINT('Ctrl Pts',(-1.08573544125307,-0.83187889150494,1.05385191525824));
#3398=CARTESIAN_POINT('Ctrl Pts',(-0.998299780142475,-0.934655883076809,
1.06253045750487));
#3399=CARTESIAN_POINT('Ctrl Pts',(-0.952685966083009,-0.981108020341267,
1.06669416484621));
#3400=CARTESIAN_POINT('Ctrl Pts',(-0.874208534799108,-1.05037514167524,
1.07356843496014));
#3401=CARTESIAN_POINT('Ctrl Pts',(-0.843351948914514,-1.07530718565557,
1.07620771903259));
#3402=CARTESIAN_POINT('Ctrl Pts',(-0.79845842317706,-1.10845894684282,1.07999483548594));
#3403=CARTESIAN_POINT('Ctrl Pts',(-0.785291300497509,-1.11782584807407,
1.08109944607787));
#3404=CARTESIAN_POINT('Ctrl Pts',(-0.762038259500069,-1.1337541040856,1.08304160395797));
#3405=CARTESIAN_POINT('Ctrl Pts',(-0.752025877316006,-1.14041998459369,
1.08387516859844));
#3406=CARTESIAN_POINT('Ctrl Pts',(-0.730998849231473,-1.1540216982819,1.08562094697105));
#3407=CARTESIAN_POINT('Ctrl Pts',(-0.719970526919759,-1.16093402797429,
1.08653390748459));
#3408=CARTESIAN_POINT('Ctrl Pts',(-0.690533193135543,-1.17880398018401,
1.08896476446125));
#3409=CARTESIAN_POINT('Ctrl Pts',(-0.671962945912466,-1.18948754599371,
1.09049214010104));
#3410=CARTESIAN_POINT('Ctrl Pts',(-0.56500683908583,-1.24771599357046,1.09925988093357));
#3411=CARTESIAN_POINT('Ctrl Pts',(-0.47185790456303,-1.28583485888557,1.10681726125845));
#3412=CARTESIAN_POINT('Ctrl Pts',(-0.330903572902713,-1.32612218781549,
1.11790517178678));
#3413=CARTESIAN_POINT('Ctrl Pts',(-0.285792030538076,-1.33657045526746,
1.12139892576925));
#3414=CARTESIAN_POINT('Ctrl Pts',(-0.214065676243491,-1.34938452167839,
1.12680055089519));
#3415=CARTESIAN_POINT('Ctrl Pts',(-0.187763169472017,-1.35329520503533,
1.1287492374207));
#3416=CARTESIAN_POINT('Ctrl Pts',(-0.151673010699197,-1.35758848340937,
1.13136552408717));
#3417=CARTESIAN_POINT('Ctrl Pts',(-0.141972225098897,-1.35863721939741,
1.13206310568842));
#3418=CARTESIAN_POINT('Ctrl Pts',(-0.125477028225057,-1.36024187879218,
1.13323876489778));
#3419=CARTESIAN_POINT('Ctrl Pts',(-0.118688322072044,-1.36085103671198,
1.13371958023493));
#3420=CARTESIAN_POINT('Ctrl Pts',(-0.104196571770856,-1.36204212105187,
1.134739240854));
#3421=CARTESIAN_POINT('Ctrl Pts',(-0.0964927459160662,-1.36260956346707,
1.13527732401677));
#3422=CARTESIAN_POINT('Ctrl Pts',(-0.0749497824999238,-1.36401273289613,
1.13677197227432));
#3423=CARTESIAN_POINT('Ctrl Pts',(-0.061101696657003,-1.36470320033262,
1.13772118002585));
#3424=CARTESIAN_POINT('Ctrl Pts',(0.0372034780668299,-1.36810524496565,
1.14439263975978));
#3425=CARTESIAN_POINT('Ctrl Pts',(0.121752283431182,-1.36318604633399,1.14978869893391));
#3426=CARTESIAN_POINT('Ctrl Pts',(0.261098416573521,-1.34200131594934,1.15885047828505));
#3427=CARTESIAN_POINT('Ctrl Pts',(0.31630198531597,-1.33007232795107,1.16248466690074));
#3428=CARTESIAN_POINT('Ctrl Pts',(0.405727375668058,-1.30486503144901,1.16860518912165));
#3429=CARTESIAN_POINT('Ctrl Pts',(0.440434414905356,-1.29356276266282,1.17104024991354));
#3430=CARTESIAN_POINT('Ctrl Pts',(0.489372418490752,-1.27542828355224,1.17458575774299));
#3431=CARTESIAN_POINT('Ctrl Pts',(0.504003801265473,-1.26971760818832,1.17566041880422));
#3432=CARTESIAN_POINT('Ctrl Pts',(0.529603649078354,-1.25921371029358,1.17756846976397));
#3433=CARTESIAN_POINT('Ctrl Pts',(0.540613836152455,-1.25452614864311,1.17839830839343));
#3434=CARTESIAN_POINT('Ctrl Pts',(0.563652892255889,-1.24435771414835,1.18015500620983));
#3435=CARTESIAN_POINT('Ctrl Pts',(0.575666573623299,-1.23884570386525,1.18108283938831));
#3436=CARTESIAN_POINT('Ctrl Pts',(0.607844845302013,-1.22351283349132,1.18360103690442));
#3437=CARTESIAN_POINT('Ctrl Pts',(0.627849877946327,-1.21336863127762,1.18520214746491));
#3438=CARTESIAN_POINT('Ctrl Pts',(0.722260749054286,-1.16253456225445,1.19293489870159));
#3439=CARTESIAN_POINT('Ctrl Pts',(0.793009068206225,-1.11547280294266,1.19928094237725));
#3440=CARTESIAN_POINT('Ctrl Pts',(0.902456238054577,-1.02696755214495,1.20992271836466));
#3441=CARTESIAN_POINT('Ctrl Pts',(0.943780540101118,-0.989125053524125,
1.21416834627533));
#3442=CARTESIAN_POINT('Ctrl Pts',(1.00329583183991,-0.927488764535791,1.22054050063554));
#3443=CARTESIAN_POINT('Ctrl Pts',(1.02322386288932,-0.905456322927489,1.22272388323281));
#3444=CARTESIAN_POINT('Ctrl Pts',(1.04896815072218,-0.875056859813829,1.22559487893615));
#3445=CARTESIAN_POINT('Ctrl Pts',(1.05543105956159,-0.86725081919667,1.22632014292951));
#3446=CARTESIAN_POINT('Ctrl Pts',(1.06613268586864,-0.854028324184944,1.22752776457364));
#3447=CARTESIAN_POINT('Ctrl Pts',(1.07041837039391,-0.848650577914439,1.22801322911521));
#3448=CARTESIAN_POINT('Ctrl Pts',(1.07933043287372,-0.837292644668275,1.22902634846271));
#3449=CARTESIAN_POINT('Ctrl Pts',(1.08394805692281,-0.831306064574237,1.22955343522473));
#3450=CARTESIAN_POINT('Ctrl Pts',(1.09664771947624,-0.814555673175179,1.23101009396719));
#3451=CARTESIAN_POINT('Ctrl Pts',(1.10462097499715,-0.803709960806694,1.23193273713203));
#3452=CARTESIAN_POINT('Ctrl Pts',(1.16443993179773,-0.719768268015663,1.23893319260093));
#3453=CARTESIAN_POINT('Ctrl Pts',(1.2091464515665,-0.641837967024095,1.24463793109827));
#3454=CARTESIAN_POINT('Ctrl Pts',(1.26795620987057,-0.511015547243028,1.25386333794568));
#3455=CARTESIAN_POINT('Ctrl Pts',(1.28709406617809,-0.460693126610454,1.25733471660028));
#3456=CARTESIAN_POINT('Ctrl Pts',(1.31055276517993,-0.386014348683778,1.26249686011757));
#3457=CARTESIAN_POINT('Ctrl Pts',(1.31726149745273,-0.362460576343731,1.26412609371639));
#3458=CARTESIAN_POINT('Ctrl Pts',(1.32838342292677,-0.319011309159441,1.26714393205334));
#3459=CARTESIAN_POINT('Ctrl Pts',(1.33299147646412,-0.299172835840265,1.26852647854059));
#3460=CARTESIAN_POINT('Ctrl Pts',(1.33977097379199,-0.266708839967383,1.2708005266587));
#3461=CARTESIAN_POINT('Ctrl Pts',(1.34221143627971,-0.254142300176839,1.2716835857127));
#3462=CARTESIAN_POINT('Ctrl Pts',(1.34661726390728,-0.229618683653578,1.27341324842383));
#3463=CARTESIAN_POINT('Ctrl Pts',(1.34860085356431,-0.217666066371998,1.2742591969321));
#3464=CARTESIAN_POINT('Ctrl Pts',(1.35294499213508,-0.189145170331141,1.27628548220772));
#3465=CARTESIAN_POINT('Ctrl Pts',(1.35516052050762,-0.172557140514531,1.27747017057894));
#3466=CARTESIAN_POINT('Ctrl Pts',(1.36174076419938,-0.115289964440575,1.28158327774038));
#3467=CARTESIAN_POINT('Ctrl Pts',(1.36458219978601,-0.0744614408658086,
1.28455666860532));
#3468=CARTESIAN_POINT('Ctrl Pts',(1.36806039770056,0.0670257218852508,1.29500164968891));
#3469=CARTESIAN_POINT('Ctrl Pts',(1.35940948633371,0.167582899848372,1.30269848514071));
#3470=CARTESIAN_POINT('Ctrl Pts',(1.33221638261792,0.304415278280409,1.31315012516));
#3471=CARTESIAN_POINT('Ctrl Pts',(1.32300708088774,0.342230901882291,1.31603197950062));
#3472=CARTESIAN_POINT('Ctrl Pts',(1.30913367781016,0.390187617103829,1.31963908805924));
#3473=CARTESIAN_POINT('Ctrl Pts',(1.30594421413549,0.400733193468631,1.32042924026901));
#3474=CARTESIAN_POINT('Ctrl Pts',(1.30050678211481,0.41795660881569,1.32171348571905));
#3475=CARTESIAN_POINT('Ctrl Pts',(1.2983341713222,0.424657514180147,1.32221156272101));
#3476=CARTESIAN_POINT('Ctrl Pts',(1.29381224996417,0.438245136255998,1.32321792442939));
#3477=CARTESIAN_POINT('Ctrl Pts',(1.2914595765778,0.445130437013794,1.32372601241792));
#3478=CARTESIAN_POINT('Ctrl Pts',(1.28504346124139,0.46342858781296,1.3250721248761));
#3479=CARTESIAN_POINT('Ctrl Pts',(1.28088292254041,0.47480703191576,1.32590484144544));
#3480=CARTESIAN_POINT('Ctrl Pts',(1.25599704284703,0.540157164712757,1.33067048288301));
#3481=CARTESIAN_POINT('Ctrl Pts',(1.23201091411976,0.5928313831814,1.33444591814982));
#3482=CARTESIAN_POINT('Ctrl Pts',(1.18003156111349,0.690096495058467,1.3415717651673));
#3483=CARTESIAN_POINT('Ctrl Pts',(1.15266315102943,0.734898206343554,1.34492331878128));
#3484=CARTESIAN_POINT('Ctrl Pts',(1.09842580315503,0.813170379170403,1.35107699943143));
#3485=CARTESIAN_POINT('Ctrl Pts',(1.07242945004472,0.847159961708913,1.35386246169437));
#3486=CARTESIAN_POINT('Ctrl Pts',(1.02523650298917,0.903203423018099,1.35872103338478));
#3487=CARTESIAN_POINT('Ctrl Pts',(1.00481548580632,0.925868202763723,1.3607676692199));
#3488=CARTESIAN_POINT('Ctrl Pts',(0.973424929579,0.958445221402814,1.3638488384095));
#3489=CARTESIAN_POINT('Ctrl Pts',(0.963024812776036,0.968894482057306,1.36485976165408));
#3490=CARTESIAN_POINT('Ctrl Pts',(0.943945671069267,0.987453081424666,1.36669820810733));
#3491=CARTESIAN_POINT('Ctrl Pts',(0.935326023762489,0.995621530342088,1.36752308807179));
#3492=CARTESIAN_POINT('Ctrl Pts',(0.916452581968859,1.01304562735979,1.369317792464));
#3493=CARTESIAN_POINT('Ctrl Pts',(0.906162778296736,1.02226012957224,1.37028920010721));
#3494=CARTESIAN_POINT('Ctrl Pts',(0.877078910421223,1.04752050574687,1.37301652726726));
#3495=CARTESIAN_POINT('Ctrl Pts',(0.85798736800867,1.06321407150413,1.37478615687274));
#3496=CARTESIAN_POINT('Ctrl Pts',(0.741794189063529,1.15355868777923,1.38544222987471));
#3497=CARTESIAN_POINT('Ctrl Pts',(0.635444600106159,1.21538316082066,1.39480632342373));
#3498=CARTESIAN_POINT('Ctrl Pts',(0.484137394908458,1.27799610643505,1.40709252244094));
#3499=CARTESIAN_POINT('Ctrl Pts',(0.445259392287595,1.29205565010245,1.41015899748468));
#3500=CARTESIAN_POINT('Ctrl Pts',(0.395105893142297,1.30765927294194,1.41395595125018));
#3501=CARTESIAN_POINT('Ctrl Pts',(0.384370512151149,1.31085497713966,1.41475960322069));
#3502=CARTESIAN_POINT('Ctrl Pts',(0.366784818952044,1.31585525358002,1.41605998066588));
#3503=CARTESIAN_POINT('Ctrl Pts',(0.359957835692098,1.3177391682049,1.41656087570821));
#3504=CARTESIAN_POINT('Ctrl Pts',(0.34613265694,1.32143877915577,1.41756689103193));
#3505=CARTESIAN_POINT('Ctrl Pts',(0.339134115492188,1.32325217594435,1.4180718811622));
#3506=CARTESIAN_POINT('Ctrl Pts',(0.320581903322071,1.32790239363983,1.41940007166375));
#3507=CARTESIAN_POINT('Ctrl Pts',(0.309004716639921,1.33064406703903,1.42021821049536));
#3508=CARTESIAN_POINT('Ctrl Pts',(0.248426050811365,1.34415681080554,1.42445065102255));
#3509=CARTESIAN_POINT('Ctrl Pts',(0.198889122788832,1.3523746814428,1.42774733026674));
#3510=CARTESIAN_POINT('Ctrl Pts',(0.0662809023176067,1.3669268119549,1.4364007878843));
#3511=CARTESIAN_POINT('Ctrl Pts',(-0.0171007684340999,1.368426015679,1.44167504131703));
#3512=CARTESIAN_POINT('Ctrl Pts',(-0.144987923195956,1.35902915175095,1.45005740647554));
#3513=CARTESIAN_POINT('Ctrl Pts',(-0.189680614389856,1.35351482330885,1.45304029687786));
#3514=CARTESIAN_POINT('Ctrl Pts',(-0.250605291534695,1.34292088147446,1.45723016631043));
#3515=CARTESIAN_POINT('Ctrl Pts',(-0.267138611501065,1.33972998270011,1.45837972152194));
#3516=CARTESIAN_POINT('Ctrl Pts',(-0.295476671902101,1.33371539090555,1.46037396341401));
#3517=CARTESIAN_POINT('Ctrl Pts',(-0.307310772708272,1.33103842172536,1.46121400475911));
#3518=CARTESIAN_POINT('Ctrl Pts',(-0.331522048115637,1.32522154884207,1.46294832692322));
#3519=CARTESIAN_POINT('Ctrl Pts',(-0.343893957955208,1.32206503168961,1.46384305637293));
#3520=CARTESIAN_POINT('Ctrl Pts',(-0.375720445324805,1.31346799894435,1.46616762533902));
#3521=CARTESIAN_POINT('Ctrl Pts',(-0.39510122864154,1.30776870250963,1.46760548940642));
#3522=CARTESIAN_POINT('Ctrl Pts',(-0.518592069877246,1.26845824971648,1.476916428314));
#3523=CARTESIAN_POINT('Ctrl Pts',(-0.618455546352899,1.22287696765016,1.48517945344773));
#3524=CARTESIAN_POINT('Ctrl Pts',(-0.74745539599868,1.14412069327667,1.4966024619638));
#3525=CARTESIAN_POINT('Ctrl Pts',(-0.782100977569658,1.12072305894729,1.49974889806064));
#3526=CARTESIAN_POINT('Ctrl Pts',(-0.829437186269884,1.08548910299477,1.50411563306687));
#3527=CARTESIAN_POINT('Ctrl Pts',(-0.843058184683076,1.07494446051572,1.50538047425985));
#3528=CARTESIAN_POINT('Ctrl Pts',(-0.866915684933313,1.0557427512455,1.50760602581046));
#3529=CARTESIAN_POINT('Ctrl Pts',(-0.877230942197576,1.04718740912945,1.50857178937316));
#3530=CARTESIAN_POINT('Ctrl Pts',(-0.893157186541404,1.03357786785068,1.51006629646821));
#3531=CARTESIAN_POINT('Ctrl Pts',(-0.89885470255575,1.02862685141355,1.51060164790513));
#3532=CARTESIAN_POINT('Ctrl Pts',(-0.90960919327487,1.0191238395641,1.51161302967644));
#3533=CARTESIAN_POINT('Ctrl Pts',(-0.914673615887704,1.01458092993267,1.51208962135287));
#3534=CARTESIAN_POINT('Ctrl Pts',(-0.925969279302745,1.00429512419505,1.51315382058671));
#3535=CARTESIAN_POINT('Ctrl Pts',(-0.932181548827975,0.998531607876709,
1.51373995789283));
#3536=CARTESIAN_POINT('Ctrl Pts',(-0.954200705440345,0.977718434680552,
1.51582235912017));
#3537=CARTESIAN_POINT('Ctrl Pts',(-0.969700927019773,0.962347423181087,
1.51729735589802));
#3538=CARTESIAN_POINT('Ctrl Pts',(-1.04549531662969,0.883493062094843,1.52459831004909));
#3539=CARTESIAN_POINT('Ctrl Pts',(-1.09992250297435,0.814723663141511,1.53014261435709));
#3540=CARTESIAN_POINT('Ctrl Pts',(-1.14737969890454,0.741266366795177,1.5357812853031));
#3541=CARTESIAN_POINT('Origin',(0.,0.,-1.10921167016993));
#3542=CARTESIAN_POINT('',(-1.14737960344529,0.741266514553124,2.25320219258599));
#3543=CARTESIAN_POINT('',(-1.14737960371854,0.741266514130168,2.135049540568));
#3544=CARTESIAN_POINT('',(-1.14737960344596,0.741266514552077,-1.10921167016993));
#3545=CARTESIAN_POINT('',(-1.36599959227551,0.0011382718177414,1.70898245993473));
#3546=CARTESIAN_POINT('Ctrl Pts',(-1.14737960344529,0.741266514553124,2.25320219258599));
#3547=CARTESIAN_POINT('Ctrl Pts',(-1.14445511162778,0.745793229568547,2.25282905037715));
#3548=CARTESIAN_POINT('Ctrl Pts',(-1.14150377684851,0.750302721850362,2.25245750693874));
#3549=CARTESIAN_POINT('Ctrl Pts',(-1.12420874842134,0.77639039027772,2.25030841753053));
#3550=CARTESIAN_POINT('Ctrl Pts',(-1.1092790965877,0.797575976318259,2.24856437172645));
#3551=CARTESIAN_POINT('Ctrl Pts',(-1.06717671624587,0.853849027793015,2.24389757279359));
#3552=CARTESIAN_POINT('Ctrl Pts',(-1.0388820822608,0.888059031968562,2.24102217132267));
#3553=CARTESIAN_POINT('Ctrl Pts',(-0.938828385019889,0.997689384824558,
2.23145678395337));
#3554=CARTESIAN_POINT('Ctrl Pts',(-0.860141974766843,1.06627218862519,2.2248422786487));
#3555=CARTESIAN_POINT('Ctrl Pts',(-0.757174265703757,1.13713775611744,2.21644016614157));
#3556=CARTESIAN_POINT('Ctrl Pts',(-0.739641422695242,1.1486190113294,2.21501867968504));
#3557=CARTESIAN_POINT('Ctrl Pts',(-0.710881183244377,1.16652086997473,2.21269702938018));
#3558=CARTESIAN_POINT('Ctrl Pts',(-0.699814171982334,1.17319354832763,2.21180601059069));
#3559=CARTESIAN_POINT('Ctrl Pts',(-0.67823343471858,1.1857913022383,2.21007205922352));
#3560=CARTESIAN_POINT('Ctrl Pts',(-0.667732550068085,1.19173605700885,2.20922992700998));
#3561=CARTESIAN_POINT('Ctrl Pts',(-0.642773149910792,1.20543261307876,2.20723122537711));
#3562=CARTESIAN_POINT('Ctrl Pts',(-0.628251309955228,1.21306444877735,2.20607062640862));
#3563=CARTESIAN_POINT('Ctrl Pts',(-0.576529716964119,1.23906847950664,2.20194303707089));
#3564=CARTESIAN_POINT('Ctrl Pts',(-0.538637322008174,1.25600414846177,2.1989290605175));
#3565=CARTESIAN_POINT('Ctrl Pts',(-0.434315959238254,1.29704014928147,2.19065726485226));
#3566=CARTESIAN_POINT('Ctrl Pts',(-0.366694825105042,1.31775443718619,2.18531753674902));
#3567=CARTESIAN_POINT('Ctrl Pts',(-0.237683512724645,1.34657143932558,2.17532002118052));
#3568=CARTESIAN_POINT('Ctrl Pts',(-0.176740113790914,1.3559175349425,2.17067545622709));
#3569=CARTESIAN_POINT('Ctrl Pts',(-0.100429649689385,1.3623856589389,2.16508987497068));
#3570=CARTESIAN_POINT('Ctrl Pts',(-0.0854693252049242,1.36340597002702,
2.16400593341543));
#3571=CARTESIAN_POINT('Ctrl Pts',(-0.062539297974867,1.36459088748245,2.16236440620136));
#3572=CARTESIAN_POINT('Ctrl Pts',(-0.0545804118632267,1.36493239419239,
2.16179829858248));
#3573=CARTESIAN_POINT('Ctrl Pts',(-0.0405439649607817,1.36541170819417,
2.16080686413368));
#3574=CARTESIAN_POINT('Ctrl Pts',(-0.03446805439255,1.36557859586381,2.16038005029851));
#3575=CARTESIAN_POINT('Ctrl Pts',(-0.0195256361898784,1.36588922526132,
2.15933594172263));
#3576=CARTESIAN_POINT('Ctrl Pts',(-0.0106585245172626,1.36598720080949,
2.15872109477129));
#3577=CARTESIAN_POINT('Ctrl Pts',(0.0186673079805364,1.36602564615178,2.15670147168563));
#3578=CARTESIAN_POINT('Ctrl Pts',(0.0391247549541757,1.3655928733285,2.15531485619726));
#3579=CARTESIAN_POINT('Ctrl Pts',(0.190191064322846,1.35899917704707,2.14518933649449));
#3580=CARTESIAN_POINT('Ctrl Pts',(0.319330730285382,1.33457366653338,2.13710173139782));
#3581=CARTESIAN_POINT('Ctrl Pts',(0.476989377424977,1.28051755840669,2.12612521357094));
#3582=CARTESIAN_POINT('Ctrl Pts',(0.510464697207438,1.26754468822479,2.12373139493531));
#3583=CARTESIAN_POINT('Ctrl Pts',(0.556668002682986,1.24751201767715,2.12031329508312));
#3584=CARTESIAN_POINT('Ctrl Pts',(0.569854819316886,1.24154378003136,2.11932436406474));
#3585=CARTESIAN_POINT('Ctrl Pts',(0.593859806606356,1.23021633044349,2.11749791709684));
#3586=CARTESIAN_POINT('Ctrl Pts',(0.604706643555955,1.22492103772442,2.11666260873504));
#3587=CARTESIAN_POINT('Ctrl Pts',(0.62677103981207,1.2137849813579,2.11494202027823));
#3588=CARTESIAN_POINT('Ctrl Pts',(0.637980473502349,1.20793079840907,2.11405634321333));
#3589=CARTESIAN_POINT('Ctrl Pts',(0.666331983982746,1.1926193596651,2.11178570868848));
#3590=CARTESIAN_POINT('Ctrl Pts',(0.683354470256632,1.18294794796436,2.1103934371967));
#3591=CARTESIAN_POINT('Ctrl Pts',(0.720117365180872,1.16100261430409,2.10732085922092));
#3592=CARTESIAN_POINT('Ctrl Pts',(0.739763900960852,1.14858406307028,2.10563590447739));
#3593=CARTESIAN_POINT('Ctrl Pts',(0.799941240925523,1.10836149643084,2.1003386900016));
#3594=CARTESIAN_POINT('Ctrl Pts',(0.839292191643858,1.07886932698377,2.09667432428138));
#3595=CARTESIAN_POINT('Ctrl Pts',(0.93590657008881,0.997970288377145,2.08718673582138));
#3596=CARTESIAN_POINT('Ctrl Pts',(0.990576504683026,0.943728996559882,2.08132325813323));
#3597=CARTESIAN_POINT('Ctrl Pts',(1.05780724003935,0.864709174676084,2.07362556634221));
#3598=CARTESIAN_POINT('Ctrl Pts',(1.07461422450469,0.843731358375023,2.07165392307157));
#3599=CARTESIAN_POINT('Ctrl Pts',(1.09684394004442,0.814242244173363,2.06899307832166));
#3600=CARTESIAN_POINT('Ctrl Pts',(1.10280676645812,0.80614782283621,2.06827374192052));
#3601=CARTESIAN_POINT('Ctrl Pts',(1.11265026385836,0.792471818039264,2.06707770370535));
#3602=CARTESIAN_POINT('Ctrl Pts',(1.11657953952223,0.786925874766503,2.06659792118672));
#3603=CARTESIAN_POINT('Ctrl Pts',(1.12479782640733,0.775140737694921,2.06558970669665));
#3604=CARTESIAN_POINT('Ctrl Pts',(1.12907661791458,0.768894863678611,2.06506191852614));
#3605=CARTESIAN_POINT('Ctrl Pts',(1.1408419043936,0.751410727626345,2.0636016142575));
#3606=CARTESIAN_POINT('Ctrl Pts',(1.14821425047003,0.740096211247739,2.06267608071435));
#3607=CARTESIAN_POINT('Ctrl Pts',(1.16469870091291,0.713957721894388,2.06057753315102));
#3608=CARTESIAN_POINT('Ctrl Pts',(1.17369791628639,0.699065055835065,2.05941030763603));
#3609=CARTESIAN_POINT('Ctrl Pts',(1.20368982138575,0.647219226519583,2.05542921262411));
#3610=CARTESIAN_POINT('Ctrl Pts',(1.22324238701773,0.609459147245914,2.05267040547807));
#3611=CARTESIAN_POINT('Ctrl Pts',(1.28608220616754,0.472847241513493,2.04297108349625));
#3612=CARTESIAN_POINT('Ctrl Pts',(1.31939023804453,0.369863666238663,2.03612735561043));
#3613=CARTESIAN_POINT('Ctrl Pts',(1.34418640305466,0.244000036540371,2.02749642267661));
#3614=CARTESIAN_POINT('Ctrl Pts',(1.34768398674082,0.223876983283783,2.02611004107536));
#3615=CARTESIAN_POINT('Ctrl Pts',(1.35263989307281,0.19101191331196,2.02383115205553));
#3616=CARTESIAN_POINT('Ctrl Pts',(1.35437229793197,0.178314022947975,2.02294715344436));
#3617=CARTESIAN_POINT('Ctrl Pts',(1.35739432598119,0.15356888944215,2.02121667279309));
#3618=CARTESIAN_POINT('Ctrl Pts',(1.35870283040466,0.141525128568418,2.02037085937764));
#3619=CARTESIAN_POINT('Ctrl Pts',(1.3614345349831,0.112832543907044,2.01834658679157));
#3620=CARTESIAN_POINT('Ctrl Pts',(1.36271274832917,0.0961722290341604,2.01716380373507));
#3621=CARTESIAN_POINT('Ctrl Pts',(1.36624012099508,0.0356611486721819,2.01283905959066));
#3622=CARTESIAN_POINT('Ctrl Pts',(1.36668019520095,-0.00826405532143513,
2.0096438025234));
#3623=CARTESIAN_POINT('Ctrl Pts',(1.36253159718782,-0.116893027612649,2.00160497196603));
#3624=CARTESIAN_POINT('Ctrl Pts',(1.35545257246667,-0.18139297887735,1.99670816699871));
#3625=CARTESIAN_POINT('Ctrl Pts',(1.33226378488829,-0.308510002733987,1.98693412446569));
#3626=CARTESIAN_POINT('Ctrl Pts',(1.31623518861522,-0.370987323090179,1.98206955718731));
#3627=CARTESIAN_POINT('Ctrl Pts',(1.29114996346084,-0.446216374935332,1.97628713545863));
#3628=CARTESIAN_POINT('Ctrl Pts',(1.28621396616711,-0.460250975101351,1.97521191144228));
#3629=CARTESIAN_POINT('Ctrl Pts',(1.27829270220742,-0.481650110489766,1.97358076019292));
#3630=CARTESIAN_POINT('Ctrl Pts',(1.27547098753056,-0.489073439714652,1.97301646647839));
#3631=CARTESIAN_POINT('Ctrl Pts',(1.27037395959123,-0.502138425591383,1.97202657597735));
#3632=CARTESIAN_POINT('Ctrl Pts',(1.26812556170161,-0.50778987546991,1.97159951783793));
#3633=CARTESIAN_POINT('Ctrl Pts',(1.26249291896948,-0.5216770070138,1.97055269496694));
#3634=CARTESIAN_POINT('Ctrl Pts',(1.25906578646912,-0.529894920079635,1.96993541218426));
#3635=CARTESIAN_POINT('Ctrl Pts',(1.24741206366561,-0.557087821974397,1.9678982489885));
#3636=CARTESIAN_POINT('Ctrl Pts',(1.23883453041687,-0.575910422932184,1.96649696448957));
#3637=CARTESIAN_POINT('Ctrl Pts',(1.1791187654265,-0.699436755686919,1.95731286834299));
#3638=CARTESIAN_POINT('Ctrl Pts',(1.11518736998412,-0.797430738654654,1.95004864461582));
#3639=CARTESIAN_POINT('Ctrl Pts',(1.00940672473423,-0.92153037274044,1.93940772411775));
#3640=CARTESIAN_POINT('Ctrl Pts',(0.977442641931367,-0.955366619199421,
1.93633043647606));
#3641=CARTESIAN_POINT('Ctrl Pts',(0.931242315930409,-0.999523050843923,
1.93200558113118));
#3642=CARTESIAN_POINT('Ctrl Pts',(0.918439378901246,-1.01129997608506,1.93081916804241));
#3643=CARTESIAN_POINT('Ctrl Pts',(0.896348343538204,-1.03085512212222,1.92878967321063));
#3644=CARTESIAN_POINT('Ctrl Pts',(0.887175099203037,-1.0387603009385,1.92795188824321));
#3645=CARTESIAN_POINT('Ctrl Pts',(0.868256268483771,-1.05463047490952,1.92623324085248));
#3646=CARTESIAN_POINT('Ctrl Pts',(0.85850329609829,-1.06258480049047,1.92535206451859));
#3647=CARTESIAN_POINT('Ctrl Pts',(0.833541829727616,-1.08237487111844,1.92310800227951));
#3648=CARTESIAN_POINT('Ctrl Pts',(0.818190646494332,-1.09402529331905,1.9217381426185));
#3649=CARTESIAN_POINT('Ctrl Pts',(0.737215259425626,-1.15282201073183,1.91456074679416));
#3650=CARTESIAN_POINT('Ctrl Pts',(0.667759053286836,-1.19439474762756,1.90855192537885));
#3651=CARTESIAN_POINT('Ctrl Pts',(0.514672635122422,-1.26847996067337,1.89571792024527));
#3652=CARTESIAN_POINT('Ctrl Pts',(0.430671548381346,-1.2994050498778,1.88890298774178));
#3653=CARTESIAN_POINT('Ctrl Pts',(0.33118371819476,-1.32531340024732,1.88143033263445));
#3654=CARTESIAN_POINT('Ctrl Pts',(0.318068581770678,-1.32852198938294,1.8804571541798));
#3655=CARTESIAN_POINT('Ctrl Pts',(0.297528369967677,-1.33322547777744,1.87895371608838));
#3656=CARTESIAN_POINT('Ctrl Pts',(0.29013517412984,-1.33485388462334,1.87841672826287));
#3657=CARTESIAN_POINT('Ctrl Pts',(0.276002095612671,-1.3378438302344,1.87739860379967));
#3658=CARTESIAN_POINT('Ctrl Pts',(0.269264930201854,-1.33921606561981,1.87691694877503));
#3659=CARTESIAN_POINT('Ctrl Pts',(0.252587846850224,-1.34248194024522,1.87573319782721));
#3660=CARTESIAN_POINT('Ctrl Pts',(0.242636466012541,-1.34431616114968,1.87503427881584));
#3661=CARTESIAN_POINT('Ctrl Pts',(0.203548499834071,-1.35107258249412,1.87231481683694));
#3662=CARTESIAN_POINT('Ctrl Pts',(0.174273649232726,-1.3551598059289,1.87033407557648));
#3663=CARTESIAN_POINT('Ctrl Pts',(0.0897290340902734,-1.36417803532848,
1.86471508731536));
#3664=CARTESIAN_POINT('Ctrl Pts',(0.0342603580363892,-1.3666967555137,1.86115068860117));
#3665=CARTESIAN_POINT('Ctrl Pts',(-0.10669439680372,-1.36450779035077,1.8520885067005));
#3666=CARTESIAN_POINT('Ctrl Pts',(-0.191855490701469,-1.35515853224204,
1.84659830138456));
#3667=CARTESIAN_POINT('Ctrl Pts',(-0.297540023977596,-1.33338990611254,
1.83936273782924));
#3668=CARTESIAN_POINT('Ctrl Pts',(-0.319384360919034,-1.3283268587274,1.83784479470394));
#3669=CARTESIAN_POINT('Ctrl Pts',(-0.353893108402389,-1.31942805768302,
1.83540545402121));
#3670=CARTESIAN_POINT('Ctrl Pts',(-0.366644000952135,-1.31594182516014,
1.83449504132481));
#3671=CARTESIAN_POINT('Ctrl Pts',(-0.390841585417997,-1.30894696148159,
1.83274891106145));
#3672=CARTESIAN_POINT('Ctrl Pts',(-0.402296723615491,-1.30547180092407,
1.83191433139074));
#3673=CARTESIAN_POINT('Ctrl Pts',(-0.428682435290027,-1.2970868770445,1.82997273787605));
#3674=CARTESIAN_POINT('Ctrl Pts',(-0.443576632824335,-1.29206916655532,
1.82886234918674));
#3675=CARTESIAN_POINT('Ctrl Pts',(-0.492803179493639,-1.27453376204648,
1.82514261085172));
#3676=CARTESIAN_POINT('Ctrl Pts',(-0.526716979709552,-1.26089653513326,
1.82249796109589));
#3677=CARTESIAN_POINT('Ctrl Pts',(-0.611624981139666,-1.22273032771862,
1.81566225591028));
#3678=CARTESIAN_POINT('Ctrl Pts',(-0.661714782062654,-1.19636409239602,
1.8114224311337));
#3679=CARTESIAN_POINT('Ctrl Pts',(-0.782157752281162,-1.12308283669411,
1.8007736761182));
#3680=CARTESIAN_POINT('Ctrl Pts',(-0.850073213613315,-1.07259657094254,
1.79434174313261));
#3681=CARTESIAN_POINT('Ctrl Pts',(-0.923271613869274,-1.00683667542334,
1.78718261223841));
#3682=CARTESIAN_POINT('Ctrl Pts',(-0.933505027874658,-0.997355987145639,
1.7861763389394));
#3683=CARTESIAN_POINT('Ctrl Pts',(-0.949132816127487,-0.982426393510283,
1.78463351231115));
#3684=CARTESIAN_POINT('Ctrl Pts',(-0.954629256730586,-0.97708633742299,
1.78408967904563));
#3685=CARTESIAN_POINT('Ctrl Pts',(-0.964945353656844,-0.966893599539856,
1.78306716901225));
#3686=CARTESIAN_POINT('Ctrl Pts',(-0.969773735305371,-0.962050764145826,
1.78258788341687));
#3687=CARTESIAN_POINT('Ctrl Pts',(-0.98150052794822,-0.950110865921041,
1.7814215923595));
#3688=CARTESIAN_POINT('Ctrl Pts',(-0.988358551429485,-0.942974725167201,
1.78073755931147));
#3689=CARTESIAN_POINT('Ctrl Pts',(-1.01410505193649,-0.915594609311967,
1.77815902620023));
#3690=CARTESIAN_POINT('Ctrl Pts',(-1.03245537780718,-0.894851206236809,
1.77629924919481));
#3691=CARTESIAN_POINT('Ctrl Pts',(-1.08183620700637,-0.835487454907541,
1.77118408703859));
#3692=CARTESIAN_POINT('Ctrl Pts',(-1.11141654365469,-0.79571525891398,1.76798778719929));
#3693=CARTESIAN_POINT('Ctrl Pts',(-1.19099869846004,-0.675588849510802,
1.75871704552248));
#3694=CARTESIAN_POINT('Ctrl Pts',(-1.23489246943862,-0.591554385658636,
1.75267571229501));
#3695=CARTESIAN_POINT('Ctrl Pts',(-1.27787244972568,-0.483200453657775,
1.74485407883813));
#3696=CARTESIAN_POINT('Ctrl Pts',(-1.28549353671963,-0.462544002193186,
1.74336282867914));
#3697=CARTESIAN_POINT('Ctrl Pts',(-1.29685978183979,-0.42928228733208,1.7409560722325));
#3698=CARTESIAN_POINT('Ctrl Pts',(-1.30092806094247,-0.416790997567367,
1.74005102802091));
#3699=CARTESIAN_POINT('Ctrl Pts',(-1.30836446014995,-0.392787810577541,
1.73830858894257));
#3700=CARTESIAN_POINT('Ctrl Pts',(-1.31176236794827,-0.381286373525596,
1.73747224168596));
#3701=CARTESIAN_POINT('Ctrl Pts',(-1.31930882341895,-0.354446978648465,
1.73551649844034));
#3702=CARTESIAN_POINT('Ctrl Pts',(-1.32334199571494,-0.339078688235434,
1.73439356533218));
#3703=CARTESIAN_POINT('Ctrl Pts',(-1.33128787542859,-0.306496525143005,
1.73200531088562));
#3704=CARTESIAN_POINT('Ctrl Pts',(-1.33513677488205,-0.289270235209399,
1.73073824013441));
#3705=CARTESIAN_POINT('Ctrl Pts',(-1.35691669726328,-0.182070234890282,
1.72282413030013));
#3706=CARTESIAN_POINT('Ctrl Pts',(-1.36607590322703,-0.0905701796946844,
1.71591966835577));
#3707=CARTESIAN_POINT('Ctrl Pts',(-1.36599952626833,0.00113764436645534,
1.70898239201339));
#3708=CARTESIAN_POINT('Ctrl Pts',(-1.3659995257529,0.0011382630833804,1.70898234521029));
#3709=CARTESIAN_POINT('Ctrl Pts',(-1.36595693287914,0.0522528482884494,
1.70511576125377));
#3710=CARTESIAN_POINT('Ctrl Pts',(-1.3630453716916,0.103328490601572,1.7012522683266));
#3711=CARTESIAN_POINT('Ctrl Pts',(-1.35497227647164,0.174423345397627,1.69595591105718));
#3712=CARTESIAN_POINT('Ctrl Pts',(-1.35221197745924,0.194669563579413,1.69445721974636));
#3713=CARTESIAN_POINT('Ctrl Pts',(-1.34761071158863,0.22356030720678,1.69233895204357));
#3714=CARTESIAN_POINT('Ctrl Pts',(-1.34613862569921,0.23225987857602,1.69170376025564));
#3715=CARTESIAN_POINT('Ctrl Pts',(-1.34341679380799,0.247448943861795,1.69060008469709));
#3716=CARTESIAN_POINT('Ctrl Pts',(-1.34220407200252,0.253944669891001,1.69012980489682));
#3717=CARTESIAN_POINT('Ctrl Pts',(-1.33978587019547,0.266395827545442,1.68923198103947));
#3718=CARTESIAN_POINT('Ctrl Pts',(-1.33858772032088,0.272352409878506,1.68880408888295));
#3719=CARTESIAN_POINT('Ctrl Pts',(-1.33572378177384,0.286114794282151,1.68781930928704));
#3720=CARTESIAN_POINT('Ctrl Pts',(-1.3340292749263,0.293914270507637,1.68726400184207));
#3721=CARTESIAN_POINT('Ctrl Pts',(-1.32893890762142,0.316392742440755,1.68567046807468));
#3722=CARTESIAN_POINT('Ctrl Pts',(-1.3253683206518,0.331031492042125,1.68464122020308));
#3723=CARTESIAN_POINT('Ctrl Pts',(-1.30471599541868,0.410002854434877,1.67912016892745));
#3724=CARTESIAN_POINT('Ctrl Pts',(-1.28318990128706,0.473087605192201,1.67482071080976));
#3725=CARTESIAN_POINT('Ctrl Pts',(-1.23091908741703,0.596061690347427,1.66622291499242));
#3726=CARTESIAN_POINT('Ctrl Pts',(-1.20018524352135,0.655748556398573,1.66193505481183));
#3727=CARTESIAN_POINT('Ctrl Pts',(-1.15937133142569,0.722453179462495,1.65680265936874));
#3728=CARTESIAN_POINT('Ctrl Pts',(-1.15343259859728,0.731897302581674,1.65606772423466));
#3729=CARTESIAN_POINT('Ctrl Pts',(-1.14737959979828,0.741266520198191,1.65532966579394));
#3730=CARTESIAN_POINT('Ctrl Pts',(-1.14737969890454,0.741266366795177,1.5357812853031));
#3731=CARTESIAN_POINT('Ctrl Pts',(-1.15979031477089,0.722056418342358,1.5372558641891));
#3732=CARTESIAN_POINT('Ctrl Pts',(-1.1717242941471,0.702525830968656,1.53873610928852));
#3733=CARTESIAN_POINT('Ctrl Pts',(-1.20824692153093,0.639228700555636,1.54349469650132));
#3734=CARTESIAN_POINT('Ctrl Pts',(-1.23090890831737,0.594421062350722,1.54680746498365));
#3735=CARTESIAN_POINT('Ctrl Pts',(-1.25804092835754,0.532533451947612,1.55138029053075));
#3736=CARTESIAN_POINT('Ctrl Pts',(-1.26472291715757,0.516463698455412,1.55256722146124));
#3737=CARTESIAN_POINT('Ctrl Pts',(-1.27557475575496,0.488891203635803,1.55460551483191));
#3738=CARTESIAN_POINT('Ctrl Pts',(-1.2799005024791,0.477451833649006,1.55545166685833));
#3739=CARTESIAN_POINT('Ctrl Pts',(-1.28786502986081,0.455503364289027,1.55707687422918));
#3740=CARTESIAN_POINT('Ctrl Pts',(-1.29153022593086,0.445004845606531,1.55785499034693));
#3741=CARTESIAN_POINT('Ctrl Pts',(-1.30081750221069,0.417320918145946,1.55990938125595));
#3742=CARTESIAN_POINT('Ctrl Pts',(-1.30622708055654,0.400067095944435,1.56119234504403));
#3743=CARTESIAN_POINT('Ctrl Pts',(-1.32640781953353,0.330921444893526,1.56634670456232));
#3744=CARTESIAN_POINT('Ctrl Pts',(-1.33843989490008,0.278287707039891,1.57030129942558));
#3745=CARTESIAN_POINT('Ctrl Pts',(-1.35980639277899,0.150391449871338,1.57996896313017));
#3746=CARTESIAN_POINT('Ctrl Pts',(-1.3660513788397,0.0747903911061498,1.58573562827326));
#3747=CARTESIAN_POINT('Ctrl Pts',(-1.36596814699086,-0.0471228114460157,
1.5949077998794));
#3748=CARTESIAN_POINT('Ctrl Pts',(-1.36359378446912,-0.093286560033794,
1.59834890468488));
#3749=CARTESIAN_POINT('Ctrl Pts',(-1.35768994075569,-0.150901693767822,
1.60254126649432));
#3750=CARTESIAN_POINT('Ctrl Pts',(-1.35634553152681,-0.162542668533079,
1.60338298691338));
#3751=CARTESIAN_POINT('Ctrl Pts',(-1.35393456769329,-0.181297817321447,
1.60472900977372));
#3752=CARTESIAN_POINT('Ctrl Pts',(-1.35296136370907,-0.188423105242078,
1.60523801726153));
#3753=CARTESIAN_POINT('Ctrl Pts',(-1.35091333127309,-0.202582827722728,
1.60624440608073));
#3754=CARTESIAN_POINT('Ctrl Pts',(-1.349839720395,-0.209617187246116,1.6067418269699));
#3755=CARTESIAN_POINT('Ctrl Pts',(-1.34690926396758,-0.22786074443878,1.60802603585138));
#3756=CARTESIAN_POINT('Ctrl Pts',(-1.34496740682321,-0.239056018908052,
1.60880835094565));
#3757=CARTESIAN_POINT('Ctrl Pts',(-1.33488735099321,-0.293152531990371,
1.61256639565084));
#3758=CARTESIAN_POINT('Ctrl Pts',(-1.32483415674441,-0.335675293826939,
1.61545300977587));
#3759=CARTESIAN_POINT('Ctrl Pts',(-1.29720218521854,-0.431728235621065,
1.62196671830796));
#3760=CARTESIAN_POINT('Ctrl Pts',(-1.278317043785,-0.484797597008448,1.62556201686632));
#3761=CARTESIAN_POINT('Ctrl Pts',(-1.22705392118097,-0.604818252505102,
1.63396583960278));
#3762=CARTESIAN_POINT('Ctrl Pts',(-1.19238366608627,-0.670586107108913,
1.63878585909729));
#3763=CARTESIAN_POINT('Ctrl Pts',(-1.14224300219914,-0.749403340349715,
1.64508482906809));
#3764=CARTESIAN_POINT('Ctrl Pts',(-1.13160028901366,-0.765379100782187,
1.64639017719041));
#3765=CARTESIAN_POINT('Ctrl Pts',(-1.11343816456112,-0.791435029837025,
1.64857052428237));
#3766=CARTESIAN_POINT('Ctrl Pts',(-1.10610966856757,-0.801645392745407,
1.64943841575736));
#3767=CARTESIAN_POINT('Ctrl Pts',(-1.09135809452728,-0.821610448686908,
1.6511632701297));
#3768=CARTESIAN_POINT('Ctrl Pts',(-1.08394252640595,-0.831369233295349,
1.65201989161256));
#3769=CARTESIAN_POINT('Ctrl Pts',(-1.06559023157837,-0.85485761231133,1.65411570260013));
#3770=CARTESIAN_POINT('Ctrl Pts',(-1.05451850304957,-0.868478413569991,
1.65536005491605));
#3771=CARTESIAN_POINT('Ctrl Pts',(-1.00981571073322,-0.921357861067739,
1.66030955055087));
#3772=CARTESIAN_POINT('Ctrl Pts',(-0.974233787236853,-0.958903249182929,
1.66409099710995));
#3773=CARTESIAN_POINT('Ctrl Pts',(-0.86947134803995,-1.05758388555974,1.6747998885656));
#3774=CARTESIAN_POINT('Ctrl Pts',(-0.796100854592957,-1.11386079793027,
1.68185536036118));
#3775=CARTESIAN_POINT('Ctrl Pts',(-0.688055432984376,-1.18056902493645,
1.69134361628397));
#3776=CARTESIAN_POINT('Ctrl Pts',(-0.657799232249098,-1.19769115466372,
1.69391094670888));
#3777=CARTESIAN_POINT('Ctrl Pts',(-0.617215340032979,-1.21865521971508,
1.6972105420373));
#3778=CARTESIAN_POINT('Ctrl Pts',(-0.607450113423378,-1.22355208291806,
1.69799384868198));
#3779=CARTESIAN_POINT('Ctrl Pts',(-0.591933664871887,-1.23110138521432,
1.69922060515191));
#3780=CARTESIAN_POINT('Ctrl Pts',(-0.5862211854455,-1.23383175928202,1.69966846371098));
#3781=CARTESIAN_POINT('Ctrl Pts',(-0.574064970579749,-1.23953853707716,
1.70061320573431));
#3782=CARTESIAN_POINT('Ctrl Pts',(-0.56761659623023,-1.24250463980213,1.70110943454097));
#3783=CARTESIAN_POINT('Ctrl Pts',(-0.550864806079229,-1.25005244223705,
1.70238661142853));
#3784=CARTESIAN_POINT('Ctrl Pts',(-0.540526990564212,-1.25455718734628,
1.70316317937415));
#3785=CARTESIAN_POINT('Ctrl Pts',(-0.491066587832421,-1.27538485387955,
1.70682919735454));
#3786=CARTESIAN_POINT('Ctrl Pts',(-0.451250238748048,-1.29001041934034,
1.70963477203816));
#3787=CARTESIAN_POINT('Ctrl Pts',(-0.309549525402229,-1.33469447777594,
1.71932757039139));
#3788=CARTESIAN_POINT('Ctrl Pts',(-0.204908935915653,-1.35471155272163,
1.72599961104273));
#3789=CARTESIAN_POINT('Ctrl Pts',(-0.0643910851198161,-1.36492277259684,
1.73529798285556));
#3790=CARTESIAN_POINT('Ctrl Pts',(-0.0296973215127461,-1.3661179093773,
1.73761756356733));
#3791=CARTESIAN_POINT('Ctrl Pts',(0.0202710338553627,-1.36593492724722,
1.74101450183231));
#3792=CARTESIAN_POINT('Ctrl Pts',(0.0355373115934018,-1.36562301102716,
1.74205980144477));
#3793=CARTESIAN_POINT('Ctrl Pts',(0.0627315591294048,-1.36461109424488,
1.74393681762103));
#3794=CARTESIAN_POINT('Ctrl Pts',(0.0746617843607647,-1.36401036991554,
1.74476542036769));
#3795=CARTESIAN_POINT('Ctrl Pts',(0.0998639783399317,-1.36240974050904,
1.74652745720307));
#3796=CARTESIAN_POINT('Ctrl Pts',(0.113132211796685,-1.36137217382533,1.74746196279611));
#3797=CARTESIAN_POINT('Ctrl Pts',(0.14916468594926,-1.35802407697473,1.75001942433337));
#3798=CARTESIAN_POINT('Ctrl Pts',(0.171888533606348,-1.35533527872778,1.75165371562096));
#3799=CARTESIAN_POINT('Ctrl Pts',(0.222848432821054,-1.34800331518345,1.75536924942726));
#3800=CARTESIAN_POINT('Ctrl Pts',(0.251027081363046,-1.34304116417229,1.75745908610927));
#3801=CARTESIAN_POINT('Ctrl Pts',(0.349556602605851,-1.32248142442519,1.76488895904059));
#3802=CARTESIAN_POINT('Ctrl Pts',(0.418805312692536,-1.30220863972253,1.77034067748926));
#3803=CARTESIAN_POINT('Ctrl Pts',(0.541995075039818,-1.25529732381879,1.78030824375599));
#3804=CARTESIAN_POINT('Ctrl Pts',(0.596412708914412,-1.23037522250698,1.78481280426713));
#3805=CARTESIAN_POINT('Ctrl Pts',(0.662110654960098,-1.19490024581714,1.79025703076469));
#3806=CARTESIAN_POINT('Ctrl Pts',(0.675079453394635,-1.18762152804031,1.79133184612928));
#3807=CARTESIAN_POINT('Ctrl Pts',(0.69478593584553,-1.17613414455211,1.79296241947197));
#3808=CARTESIAN_POINT('Ctrl Pts',(0.701609658132619,-1.17207632782718,1.79352653769146));
#3809=CARTESIAN_POINT('Ctrl Pts',(0.713596933441673,-1.16480573107767,1.7945161320364));
#3810=CARTESIAN_POINT('Ctrl Pts',(0.718774762820622,-1.1616177586051,1.79494306854411));
#3811=CARTESIAN_POINT('Ctrl Pts',(0.731479386535359,-1.1536780872011,1.79598958265653));
#3812=CARTESIAN_POINT('Ctrl Pts',(0.738981301846574,-1.14888723041647,1.79660667987652));
#3813=CARTESIAN_POINT('Ctrl Pts',(0.763749689625065,-1.13272670273973,1.7986431244583));
#3814=CARTESIAN_POINT('Ctrl Pts',(0.780805734832701,-1.12103786147678,1.80004388997056));
#3815=CARTESIAN_POINT('Ctrl Pts',(0.892143391326122,-1.04096152236886,1.80922410355532));
#3816=CARTESIAN_POINT('Ctrl Pts',(0.977618909325426,-0.961138804459532,
1.81648530253784));
#3817=CARTESIAN_POINT('Ctrl Pts',(1.08164744551156,-0.83556217078932,1.82712605079926));
#3818=CARTESIAN_POINT('Ctrl Pts',(1.10950380236102,-0.798201716139281,1.83020690364902));
#3819=CARTESIAN_POINT('Ctrl Pts',(1.1450686222001,-0.745034559755364,1.83453561316257));
#3820=CARTESIAN_POINT('Ctrl Pts',(1.15446366260434,-0.730391847358991,1.83572214500001));
#3821=CARTESIAN_POINT('Ctrl Pts',(1.16991844935883,-0.705261231545455,1.8377516054818));
#3822=CARTESIAN_POINT('Ctrl Pts',(1.17612315953832,-0.694864648806059,1.83858923352938));
#3823=CARTESIAN_POINT('Ctrl Pts',(1.18849137527153,-0.673500187716444,1.84030734340655));
#3824=CARTESIAN_POINT('Ctrl Pts',(1.19464317604421,-0.662526916569924,1.84118813647998));
#3825=CARTESIAN_POINT('Ctrl Pts',(1.20982561328582,-0.634546101434539,1.84343074348033));
#3826=CARTESIAN_POINT('Ctrl Pts',(1.21864953639005,-0.617430166024213,1.84479951679691));
#3827=CARTESIAN_POINT('Ctrl Pts',(1.26240783761792,-0.52795654813841,1.85194305323672));
#3828=CARTESIAN_POINT('Ctrl Pts',(1.29126466282779,-0.452817109349181,1.85791664565611));
#3829=CARTESIAN_POINT('Ctrl Pts',(1.33807042273222,-0.289148431385013,1.8707611013959));
#3830=CARTESIAN_POINT('Ctrl Pts',(1.35419800661244,-0.20047237521511,1.87762446816413));
#3831=CARTESIAN_POINT('Ctrl Pts',(1.36258439726296,-0.0974680645364525,
1.88513511386748));
#3832=CARTESIAN_POINT('Ctrl Pts',(1.36347662556989,-0.0840701443760326,
1.88610280800168));
#3833=CARTESIAN_POINT('Ctrl Pts',(1.36456192063752,-0.0631174811284687,
1.88759961860249));
#3834=CARTESIAN_POINT('Ctrl Pts',(1.36489007738468,-0.0555709935379551,
1.88813537441347));
#3835=CARTESIAN_POINT('Ctrl Pts',(1.36539748947144,-0.0411464116040726,
1.88915255846849));
#3836=CARTESIAN_POINT('Ctrl Pts',(1.36558740485288,-0.0342691310991905,
1.88963448772472));
#3837=CARTESIAN_POINT('Ctrl Pts',(1.36592892455662,-0.0172405652041577,
1.89082081033994));
#3838=CARTESIAN_POINT('Ctrl Pts',(1.36601933983523,-0.00708822082055721,
1.89152199185013));
#3839=CARTESIAN_POINT('Ctrl Pts',(1.36592957592852,0.0329230015985243,1.89426470334038));
#3840=CARTESIAN_POINT('Ctrl Pts',(1.36488361542284,0.0627737554192573,1.89626555151596));
#3841=CARTESIAN_POINT('Ctrl Pts',(1.35902933441631,0.148964591954679,1.90197259659998));
#3842=CARTESIAN_POINT('Ctrl Pts',(1.35170167793814,0.205072090262172,1.90560218676086));
#3843=CARTESIAN_POINT('Ctrl Pts',(1.32489148691063,0.343041396830687,1.91463695028003));
#3844=CARTESIAN_POINT('Ctrl Pts',(1.30129239579022,0.423852524379415,1.92003701397138));
#3845=CARTESIAN_POINT('Ctrl Pts',(1.26217639524908,0.522848184741809,1.92717449023204));
#3846=CARTESIAN_POINT('Ctrl Pts',(1.25341822028006,0.543509105631328,1.92869355971991));
#3847=CARTESIAN_POINT('Ctrl Pts',(1.23869791154941,0.575984587447113,1.93113411475356));
#3848=CARTESIAN_POINT('Ctrl Pts',(1.23306590808666,0.587944900843358,1.93204459117415));
#3849=CARTESIAN_POINT('Ctrl Pts',(1.22200704329029,0.610571838066217,1.93379045723406));
#3850=CARTESIAN_POINT('Ctrl Pts',(1.2166118329917,0.621252617789063,1.93462470437699));
#3851=CARTESIAN_POINT('Ctrl Pts',(1.20381411363676,0.645781793014084,1.93656493148445));
#3852=CARTESIAN_POINT('Ctrl Pts',(1.19631187273207,0.659575932750349,1.9376742749992));
#3853=CARTESIAN_POINT('Ctrl Pts',(1.17060348511937,0.704963080259483,1.94138719796597));
#3854=CARTESIAN_POINT('Ctrl Pts',(1.15137173673887,0.735953908320155,1.9440259052185));
#3855=CARTESIAN_POINT('Ctrl Pts',(1.09931637092046,0.812794978268084,1.95084060671881));
#3856=CARTESIAN_POINT('Ctrl Pts',(1.0648532977811,0.857448858384555,1.95506497107772));
#3857=CARTESIAN_POINT('Ctrl Pts',(0.97198001816735,0.963521857650683,1.96571313500633));
#3858=CARTESIAN_POINT('Ctrl Pts',(0.910424313975098,1.02188509508412,1.97216107519307));
#3859=CARTESIAN_POINT('Ctrl Pts',(0.832965640074657,1.0827354817752,1.9793286607213));
#3860=CARTESIAN_POINT('Ctrl Pts',(0.821942712968765,1.0911269838918,1.9803281836888));
#3861=CARTESIAN_POINT('Ctrl Pts',(0.804579128565239,1.10393299191961,1.98186880073366));
#3862=CARTESIAN_POINT('Ctrl Pts',(0.798325792568124,1.10846360387413,1.98241696122259));
#3863=CARTESIAN_POINT('Ctrl Pts',(0.786480772432027,1.11689321525958,1.98344228041507));
#3864=CARTESIAN_POINT('Ctrl Pts',(0.780898070023141,1.12080358050575,1.9839201165184));
#3865=CARTESIAN_POINT('Ctrl Pts',(0.767249847624264,1.13021190000869,1.98507567572538));
#3866=CARTESIAN_POINT('Ctrl Pts',(0.759154260638993,1.13566548340149,1.98575056024861));
#3867=CARTESIAN_POINT('Ctrl Pts',(0.728766168739874,1.15566621548915,1.98824761649419));
#3868=CARTESIAN_POINT('Ctrl Pts',(0.706106970783736,1.16964853497552,1.99003782705513));
#3869=CARTESIAN_POINT('Ctrl Pts',(0.642893686895688,1.20614844093588,1.99488014891978));
#3870=CARTESIAN_POINT('Ctrl Pts',(0.601578013534652,1.2272778063075,1.99788046743877));
#3871=CARTESIAN_POINT('Ctrl Pts',(0.467865890469464,1.2872814860074,2.0073183310386));
#3872=CARTESIAN_POINT('Ctrl Pts',(0.372241759951797,1.31811454171755,2.01369950851955));
#3873=CARTESIAN_POINT('Ctrl Pts',(0.253102911053024,1.34251805575169,2.02186737679989));
#3874=CARTESIAN_POINT('Ctrl Pts',(0.231998414634837,1.34632554247638,2.0233209684485));
#3875=CARTESIAN_POINT('Ctrl Pts',(0.19795103780313,1.35164376901594,2.02568160787958));
#3876=CARTESIAN_POINT('Ctrl Pts',(0.185060443848407,1.35346891495904,2.0265789113278));
#3877=CARTESIAN_POINT('Ctrl Pts',(0.160216336675511,1.35662498191178,2.02831610033631));
#3878=CARTESIAN_POINT('Ctrl Pts',(0.148267424505036,1.35798283150136,2.02915506856913));
#3879=CARTESIAN_POINT('Ctrl Pts',(0.120237313492564,1.36079376586956,2.03113198252251));
#3880=CARTESIAN_POINT('Ctrl Pts',(0.104145496440448,1.36211980409619,2.03227371218323));
#3881=CARTESIAN_POINT('Ctrl Pts',(0.0485481285201941,1.36571034984221,2.03624365673629));
#3882=CARTESIAN_POINT('Ctrl Pts',(0.00897336138771308,1.36654330793505,
2.0391141343248));
#3883=CARTESIAN_POINT('Ctrl Pts',(-0.0953385835039811,1.36420765506473,
2.04679903771023));
#3884=CARTESIAN_POINT('Ctrl Pts',(-0.159907984497101,1.35815315521377,2.0516805162905));
#3885=CARTESIAN_POINT('Ctrl Pts',(-0.293053759337824,1.33604046037419,2.06188999303428));
#3886=CARTESIAN_POINT('Ctrl Pts',(-0.361325348218605,1.3192157736059,2.067206460136));
#3887=CARTESIAN_POINT('Ctrl Pts',(-0.442124991239913,1.29255659660808,2.07341046631218));
#3888=CARTESIAN_POINT('Ctrl Pts',(-0.456168240006155,1.28766752133638,2.07448514832784));
#3889=CARTESIAN_POINT('Ctrl Pts',(-0.477582906572202,1.27981779329343,2.07611556313191));
#3890=CARTESIAN_POINT('Ctrl Pts',(-0.485012534794449,1.27702069904108,2.07667965378334));
#3891=CARTESIAN_POINT('Ctrl Pts',(-0.498089499043235,1.27196691244003,2.07766922508382));
#3892=CARTESIAN_POINT('Ctrl Pts',(-0.503746533230021,1.26973714124726,2.07809616572091));
#3893=CARTESIAN_POINT('Ctrl Pts',(-0.517648016565792,1.26415021374995,2.07914272288182));
#3894=CARTESIAN_POINT('Ctrl Pts',(-0.525874841512708,1.2607501314389,2.07975985848602));
#3895=CARTESIAN_POINT('Ctrl Pts',(-0.55309880478091,1.24918582642946,2.08179657972262));
#3896=CARTESIAN_POINT('Ctrl Pts',(-0.571944739123921,1.24067032008993,2.08319757661226));
#3897=CARTESIAN_POINT('Ctrl Pts',(-0.695623101784743,1.18136886689752,2.092378884129));
#3898=CARTESIAN_POINT('Ctrl Pts',(-0.793791368570804,1.11777680002107,2.09964087603822));
#3899=CARTESIAN_POINT('Ctrl Pts',(-0.918239182809894,1.0124034241297,2.11028161895936));
#3900=CARTESIAN_POINT('Ctrl Pts',(-0.952208118340535,0.980521758778849,
2.11336147694505));
#3901=CARTESIAN_POINT('Ctrl Pts',(-0.996540189408266,0.934433651826953,
2.11768905763102));
#3902=CARTESIAN_POINT('Ctrl Pts',(-1.00835835459753,0.921668043105,2.11887550204496));
#3903=CARTESIAN_POINT('Ctrl Pts',(-1.02798277302616,0.899641037135389,2.12090485927624));
#3904=CARTESIAN_POINT('Ctrl Pts',(-1.03591567987304,0.890494955191887,2.12174247284238));
#3905=CARTESIAN_POINT('Ctrl Pts',(-1.05184157065017,0.871632704057748,2.12346059308518));
#3906=CARTESIAN_POINT('Ctrl Pts',(-1.05982396606316,0.861909161563552,2.12434141147899));
#3907=CARTESIAN_POINT('Ctrl Pts',(-1.06844721718715,0.85110404404337,2.12531527796639));
#3908=CARTESIAN_POINT('Ctrl Pts',(-1.06922240375786,0.850129990640251,2.12540302600043));
#3909=CARTESIAN_POINT('Ctrl Pts',(-1.07074439071018,0.848212177559546,2.12557570809491));
#3910=CARTESIAN_POINT('Ctrl Pts',(-1.07149127765662,0.847268487722126,2.12566063868679));
#3911=CARTESIAN_POINT('Ctrl Pts',(-1.07299582710629,0.845362321983506,2.12583210977877));
#3912=CARTESIAN_POINT('Ctrl Pts',(-1.0737534439973,0.84439981164343,2.12591865193961));
#3913=CARTESIAN_POINT('Ctrl Pts',(-1.07531538819257,0.842409946713103,2.12609748159864));
#3914=CARTESIAN_POINT('Ctrl Pts',(-1.0761195399428,0.841382456518589,2.12618977574813));
#3915=CARTESIAN_POINT('Ctrl Pts',(-1.07781382997867,0.839211206101592,2.12638471021053));
#3916=CARTESIAN_POINT('Ctrl Pts',(-1.0787036220003,0.838067178926906,2.12648736366916));
#3917=CARTESIAN_POINT('Ctrl Pts',(-1.08061786038151,0.835597897090972,2.12670880997662));
#3918=CARTESIAN_POINT('Ctrl Pts',(-1.08164169217297,0.834272171121222,2.12682762609339));
#3919=CARTESIAN_POINT('Ctrl Pts',(-1.08388919555604,0.831350861566436,2.12708927897632));
#3920=CARTESIAN_POINT('Ctrl Pts',(-1.08511178592161,0.829754454792491,2.12723215646491));
#3921=CARTESIAN_POINT('Ctrl Pts',(-1.10677711903415,0.801335005219596,2.12977378257878));
#3922=CARTESIAN_POINT('Ctrl Pts',(-1.1262214474394,0.773768885370967,2.13220954871428));
#3923=CARTESIAN_POINT('Ctrl Pts',(-1.14554557903622,0.744099572673573,2.13480218152378));
#3924=CARTESIAN_POINT('Ctrl Pts',(-1.14646391675869,0.742683872827873,2.13492582294454));
#3925=CARTESIAN_POINT('Ctrl Pts',(-1.14737960371854,0.741266514130168,2.135049540568));
#3926=CARTESIAN_POINT('Origin',(0.,0.,-1.10921167016993));
#3927=CARTESIAN_POINT('',(-1.14737960323804,0.741266514873919,2.85523392653093));
#3928=CARTESIAN_POINT('',(-1.1473796034465,0.741266514551254,2.73724103392041));
#3929=CARTESIAN_POINT('',(-1.14737960344596,0.741266514552077,-1.10921167016993));
#3930=CARTESIAN_POINT('Ctrl Pts',(-1.14737960323804,0.741266514873919,2.85523392653093));
#3931=CARTESIAN_POINT('Ctrl Pts',(-1.14653083367509,0.742580294553478,2.85511804770569));
#3932=CARTESIAN_POINT('Ctrl Pts',(-1.14567979272863,0.743892639525033,2.85500210777706));
#3933=CARTESIAN_POINT('Ctrl Pts',(-1.08129912223108,0.842798095947521,2.84625010182325));
#3934=CARTESIAN_POINT('Ctrl Pts',(-1.00556037785319,0.931859337276389,2.83727237967739));
#3935=CARTESIAN_POINT('Ctrl Pts',(-0.904171665713376,1.02413687155565,2.82718320205455));
#3936=CARTESIAN_POINT('Ctrl Pts',(-0.88857982526168,1.03769395230865,2.82567864389195));
#3937=CARTESIAN_POINT('Ctrl Pts',(-0.865838834274635,1.05657858949772,2.82355704704619));
#3938=CARTESIAN_POINT('Ctrl Pts',(-0.858936549220571,1.06219735365717,2.82292237596522));
#3939=CARTESIAN_POINT('Ctrl Pts',(-0.847225704348335,1.07154169035215,2.82186172145223));
#3940=CARTESIAN_POINT('Ctrl Pts',(-0.842446466710632,1.07530318719371,2.82143333968576));
#3941=CARTESIAN_POINT('Ctrl Pts',(-0.831367093837753,1.08390398893679,2.82045061638249));
#3942=CARTESIAN_POINT('Ctrl Pts',(-0.825049645711192,1.08872043795629,2.81989781566776));
#3943=CARTESIAN_POINT('Ctrl Pts',(-0.806772771386808,1.10240434426697,2.81831890463741));
#3944=CARTESIAN_POINT('Ctrl Pts',(-0.794709520561203,1.11113206496247,2.81730152337101));
#3945=CARTESIAN_POINT('Ctrl Pts',(-0.725947839445159,1.15918801575539,2.81162516326725));
#3946=CARTESIAN_POINT('Ctrl Pts',(-0.666469695326698,1.19437745373598,2.80717474218855));
#3947=CARTESIAN_POINT('Ctrl Pts',(-0.545782316230265,1.25394461302342,2.79851780933413));
#3948=CARTESIAN_POINT('Ctrl Pts',(-0.484973822923106,1.27869279043026,2.79432057740742));
#3949=CARTESIAN_POINT('Ctrl Pts',(-0.38473775364833,1.31130479169281,2.78739934982316));
#3950=CARTESIAN_POINT('Ctrl Pts',(-0.346332381085573,1.32196702860901,2.78474801470412));
#3951=CARTESIAN_POINT('Ctrl Pts',(-0.29174828390894,1.33457892848013,2.78094656848575));
#3952=CARTESIAN_POINT('Ctrl Pts',(-0.275915121172672,1.33794199654319,2.77984014151979));
#3953=CARTESIAN_POINT('Ctrl Pts',(-0.248212421900609,1.34331359457473,2.77789576258713));
#3954=CARTESIAN_POINT('Ctrl Pts',(-0.236368940982478,1.34544807681726,2.77706181840495));
#3955=CARTESIAN_POINT('Ctrl Pts',(-0.211667885710037,1.34956360255032,2.77531618479486));
#3956=CARTESIAN_POINT('Ctrl Pts',(-0.198807170403423,1.35151799819961,2.77440375957859));
#3957=CARTESIAN_POINT('Ctrl Pts',(-0.164741464188319,1.35619809929917,2.77197660164922));
#3958=CARTESIAN_POINT('Ctrl Pts',(-0.143497774679793,1.35861007357041,2.77045244433473));
#3959=CARTESIAN_POINT('Ctrl Pts',(-0.0218578296249289,1.36953623210188,
2.76166010379382));
#3960=CARTESIAN_POINT('Ctrl Pts',(0.0791646933984834,1.36741850453304,2.75407190559131));
#3961=CARTESIAN_POINT('Ctrl Pts',(0.224687844743802,1.34818165795214,2.7429696788253));
#3962=CARTESIAN_POINT('Ctrl Pts',(0.270027868009202,1.33983722671712,2.73949165813805));
#3963=CARTESIAN_POINT('Ctrl Pts',(0.340661513831219,1.3231057106918,2.73411069261342));
#3964=CARTESIAN_POINT('Ctrl Pts',(0.366280154942863,1.31624391887726,2.73216725338979));
#3965=CARTESIAN_POINT('Ctrl Pts',(0.401023953141729,1.30584487022744,2.72955664218566));
#3966=CARTESIAN_POINT('Ctrl Pts',(0.410333402673673,1.30294955730597,2.72885964909161));
#3967=CARTESIAN_POINT('Ctrl Pts',(0.426097400193815,1.29786110851335,2.72768459000048));
#3968=CARTESIAN_POINT('Ctrl Pts',(0.432567842298856,1.29571892080389,2.72720379472912));
#3969=CARTESIAN_POINT('Ctrl Pts',(0.446343354796048,1.29104352380714,2.72618368530728));
#3970=CARTESIAN_POINT('Ctrl Pts',(0.453643340125955,1.28849660383361,2.72564513956115));
#3971=CARTESIAN_POINT('Ctrl Pts',(0.473996909333182,1.28120094508637,2.72414825045489));
#3972=CARTESIAN_POINT('Ctrl Pts',(0.487000671769003,1.27631473961987,2.72319729750435));
#3973=CARTESIAN_POINT('Ctrl Pts',(0.593568526577657,1.23440552707315,2.71543106598301));
#3974=CARTESIAN_POINT('Ctrl Pts',(0.682866157069123,1.18734157676016,2.70907912829546));
#3975=CARTESIAN_POINT('Ctrl Pts',(0.812638308661457,1.09941917507033,2.69897093736381));
#3976=CARTESIAN_POINT('Ctrl Pts',(0.857098405444911,1.06512207295732,2.69532373186021));
#3977=CARTESIAN_POINT('Ctrl Pts',(0.918910277749296,1.01105745337468,2.68984650770516));
#3978=CARTESIAN_POINT('Ctrl Pts',(0.938004193973587,0.993368643588955,2.68809212479594));
#3979=CARTESIAN_POINT('Ctrl Pts',(0.966523127121389,0.965392684445844,2.68536452447334));
#3980=CARTESIAN_POINT('Ctrl Pts',(0.976315858642235,0.955487995899881,2.68440739368148));
#3981=CARTESIAN_POINT('Ctrl Pts',(0.994171365316706,0.936867237025232,2.68262235359033));
#3982=CARTESIAN_POINT('Ctrl Pts',(1.00227532184794,0.928192376108285,2.68179630836139));
#3983=CARTESIAN_POINT('Ctrl Pts',(1.02009555147639,0.908611242047245,2.67994323585171));
#3984=CARTESIAN_POINT('Ctrl Pts',(1.02975190157295,0.897652669553067,2.6789138718951));
#3985=CARTESIAN_POINT('Ctrl Pts',(1.05418312195726,0.86901367283767,2.67624219348566));
#3986=CARTESIAN_POINT('Ctrl Pts',(1.06868919174816,0.851111107294155,2.67458960543642));
#3987=CARTESIAN_POINT('Ctrl Pts',(1.14563030251882,0.751085047189641,2.66544592974648));
#3988=CARTESIAN_POINT('Ctrl Pts',(1.19905248462926,0.662468202727034,2.65763112537259));
#3989=CARTESIAN_POINT('Ctrl Pts',(1.25841661819214,0.532823606047787,2.64686151420327));
#3990=CARTESIAN_POINT('Ctrl Pts',(1.27328480550014,0.496245440073111,2.64389413711922));
#3991=CARTESIAN_POINT('Ctrl Pts',(1.29463872594448,0.436401215179274,2.63919711517297));
#3992=CARTESIAN_POINT('Ctrl Pts',(1.30212846322436,0.413517937812812,2.6374371023121));
#3993=CARTESIAN_POINT('Ctrl Pts',(1.3117019096116,0.381422072786795,2.63502876280897));
#3994=CARTESIAN_POINT('Ctrl Pts',(1.31430054928348,0.372369139817996,2.63435604875521));
#3995=CARTESIAN_POINT('Ctrl Pts',(1.3186059736694,0.356763396622772,2.63320850667838));
#3996=CARTESIAN_POINT('Ctrl Pts',(1.32035800274831,0.350223624963691,2.63273127191815));
#3997=CARTESIAN_POINT('Ctrl Pts',(1.32405013281965,0.336020426347164,2.63170290125094));
#3998=CARTESIAN_POINT('Ctrl Pts',(1.32597244063254,0.328352821948098,2.63115272926185));
#3999=CARTESIAN_POINT('Ctrl Pts',(1.3312793380025,0.306377970144358,2.62958908472244));
#4000=CARTESIAN_POINT('Ctrl Pts',(1.33449977867376,0.292031711510687,2.62858408434089));
#4001=CARTESIAN_POINT('Ctrl Pts',(1.35156907257844,0.209801686377302,2.622899060866));
#4002=CARTESIAN_POINT('Ctrl Pts',(1.36047079662161,0.140986488007043,2.61843053621497));
#4003=CARTESIAN_POINT('Ctrl Pts',(1.36755948431215,0.00628367727474066,
2.60975413098043));
#4004=CARTESIAN_POINT('Ctrl Pts',(1.36628402753273,-0.0593785824087688,
2.60555549584965));
#4005=CARTESIAN_POINT('Ctrl Pts',(1.35665923117047,-0.164376839088424,2.59863230686157));
#4006=CARTESIAN_POINT('Ctrl Pts',(1.35128714060748,-0.20387894757638,2.59598047176616));
#4007=CARTESIAN_POINT('Ctrl Pts',(1.34131611813841,-0.259015603627945,2.59217843645943));
#4008=CARTESIAN_POINT('Ctrl Pts',(1.33815280691061,-0.274890959745322,2.59107193960064));
#4009=CARTESIAN_POINT('Ctrl Pts',(1.33214718152976,-0.302464394902681,2.58912748040693));
#4010=CARTESIAN_POINT('Ctrl Pts',(1.32943090435045,-0.314188284180502,2.58829352687372));
#4011=CARTESIAN_POINT('Ctrl Pts',(1.32345702899145,-0.338506561817742,2.58654791507393));
#4012=CARTESIAN_POINT('Ctrl Pts',(1.32017372444422,-0.351093316030731,2.58563552151683));
#4013=CARTESIAN_POINT('Ctrl Pts',(1.31102089210131,-0.384235818310119,2.58320854854815));
#4014=CARTESIAN_POINT('Ctrl Pts',(1.30484793580201,-0.404703245400948,2.58168454714169));
#4015=CARTESIAN_POINT('Ctrl Pts',(1.26684375796151,-0.520785657905018,2.57289112198094));
#4016=CARTESIAN_POINT('Ctrl Pts',(1.2249937366015,-0.612775905079113,2.56530154968322));
#4017=CARTESIAN_POINT('Ctrl Pts',(1.14984214518684,-0.738877928697974,2.55419870524363));
#4018=CARTESIAN_POINT('Ctrl Pts',(1.1242746112331,-0.777228784848023,2.5507214052825));
#4019=CARTESIAN_POINT('Ctrl Pts',(1.08101523291244,-0.835502772238854,2.54534139034468));
#4020=CARTESIAN_POINT('Ctrl Pts',(1.06459571506041,-0.85632645458842,2.54339819579169));
#4021=CARTESIAN_POINT('Ctrl Pts',(1.04132313674688,-0.884136388110229,2.54078785252486));
#4022=CARTESIAN_POINT('Ctrl Pts',(1.03498691711868,-0.891545356915325,2.54009089026485));
#4023=CARTESIAN_POINT('Ctrl Pts',(1.02408682544234,-0.904018044367269,2.53891586647293));
#4024=CARTESIAN_POINT('Ctrl Pts',(1.01956347714145,-0.909116480513805,2.53843507607641));
#4025=CARTESIAN_POINT('Ctrl Pts',(1.0098277536541,-0.919925911034869,2.53741495782153));
#4026=CARTESIAN_POINT('Ctrl Pts',(1.00460478726949,-0.925626816074157,2.53687639859961));
#4027=CARTESIAN_POINT('Ctrl Pts',(0.989863275108719,-0.941445513130695,
2.53537943278435));
#4028=CARTESIAN_POINT('Ctrl Pts',(0.980238094300213,-0.951463227465583,
2.53442841780528));
#4029=CARTESIAN_POINT('Ctrl Pts',(0.911199052646548,-1.02115783906046,2.52777524921006));
#4030=CARTESIAN_POINT('Ctrl Pts',(0.846523750799378,-1.07538286515854,2.52239677369653));
#4031=CARTESIAN_POINT('Ctrl Pts',(0.730728034773992,-1.15550601540192,2.5133437866314));
#4032=CARTESIAN_POINT('Ctrl Pts',(0.682244625442632,-1.18477816941618,2.50969993362544));
#4033=CARTESIAN_POINT('Ctrl Pts',(0.599684707391595,-1.22787228080641,2.50356532420787));
#4034=CARTESIAN_POINT('Ctrl Pts',(0.566617558370231,-1.24347749004527,2.50112616916176));
#4035=CARTESIAN_POINT('Ctrl Pts',(0.518494485839277,-1.26386966004305,2.49757562455074));
#4036=CARTESIAN_POINT('Ctrl Pts',(0.503918161040141,-1.2697517482131,2.49650016041877));
#4037=CARTESIAN_POINT('Ctrl Pts',(0.47806749438124,-1.27966822603475,2.49459100468783));
#4038=CARTESIAN_POINT('Ctrl Pts',(0.466835355641053,-1.28380840968344,2.49376087358823));
#4039=CARTESIAN_POINT('Ctrl Pts',(0.443089456702582,-1.29220835903634,2.49200387346505));
#4040=CARTESIAN_POINT('Ctrl Pts',(0.430565434103959,-1.29643514879154,2.49107603382018));
#4041=CARTESIAN_POINT('Ctrl Pts',(0.396640576764781,-1.30733881567284,2.48855860778375));
#4042=CARTESIAN_POINT('Ctrl Pts',(0.375134296022604,-1.31367145098252,2.48695829136088));
#4043=CARTESIAN_POINT('Ctrl Pts',(0.270718389550387,-1.34164419845191,2.47916284681783));
#4044=CARTESIAN_POINT('Ctrl Pts',(0.186063956604697,-1.35597693372624,2.4727482282083));
#4045=CARTESIAN_POINT('Ctrl Pts',(0.045444893860012,-1.36636517156687,2.46208671552133));
#4046=CARTESIAN_POINT('Ctrl Pts',(-0.00994806838753257,-1.36708468047476,
2.45789025712734));
#4047=CARTESIAN_POINT('Ctrl Pts',(-0.0947104808179618,-1.36303220484456,
2.45158030429225));
#4048=CARTESIAN_POINT('Ctrl Pts',(-0.124136373990518,-1.36066796622916,
2.44941103810261));
#4049=CARTESIAN_POINT('Ctrl Pts',(-0.163514733513941,-1.35621577324427,
2.44655511761264));
#4050=CARTESIAN_POINT('Ctrl Pts',(-0.173552098013563,-1.35496788766778,
2.44583129909112));
#4051=CARTESIAN_POINT('Ctrl Pts',(-0.190387088375231,-1.35268474297834,
2.44462525296046));
#4052=CARTESIAN_POINT('Ctrl Pts',(-0.197192303938863,-1.35170945889443,
2.44413993900791));
#4053=CARTESIAN_POINT('Ctrl Pts',(-0.211477117431756,-1.34955205926757,
2.44312617616002));
#4054=CARTESIAN_POINT('Ctrl Pts',(-0.218954692177259,-1.34835906999399,
2.44259830688548));
#4055=CARTESIAN_POINT('Ctrl Pts',(-0.239744179492438,-1.34486475816824,
2.44113752635005));
#4056=CARTESIAN_POINT('Ctrl Pts',(-0.253032855709848,-1.3424279860794,2.4402116050373));
#4057=CARTESIAN_POINT('Ctrl Pts',(-0.353784510116791,-1.32240361846912,
2.43323594435198));
#4058=CARTESIAN_POINT('Ctrl Pts',(-0.439383386724051,-1.2964803885036,2.42755539874409));
#4059=CARTESIAN_POINT('Ctrl Pts',(-0.59657267375393,-1.23150088251039,2.41661585361514));
#4060=CARTESIAN_POINT('Ctrl Pts',(-0.6683951088256,-1.19404319213079,2.41138729132463));
#4061=CARTESIAN_POINT('Ctrl Pts',(-0.752710411757752,-1.14006773181688,
2.40463765087472));
#4062=CARTESIAN_POINT('Ctrl Pts',(-0.768718780379926,-1.12933554469368,
2.40332722943582));
#4063=CARTESIAN_POINT('Ctrl Pts',(-0.794797134244905,-1.11104091229297,
2.4011405766563));
#4064=CARTESIAN_POINT('Ctrl Pts',(-0.804999453118168,-1.10367126249358,
2.40027153611508));
#4065=CARTESIAN_POINT('Ctrl Pts',(-0.82481531285194,-1.08893633003308,2.3985558035106));
#4066=CARTESIAN_POINT('Ctrl Pts',(-0.834435630017448,-1.08158207913001,
2.39770958675804));
#4067=CARTESIAN_POINT('Ctrl Pts',(-0.857633544623524,-1.06335471310932,
2.39563568753407));
#4068=CARTESIAN_POINT('Ctrl Pts',(-0.871103357674404,-1.05234853233427,
2.39440290321733));
#4069=CARTESIAN_POINT('Ctrl Pts',(-0.919804868299132,-1.01097874854762,
2.38983681183424));
#4070=CARTESIAN_POINT('Ctrl Pts',(-0.953686153425763,-0.979081654086912,
2.38644357172854));
#4071=CARTESIAN_POINT('Ctrl Pts',(-1.0665467465238,-0.861404780124572,2.3743526597629));
#4072=CARTESIAN_POINT('Ctrl Pts',(-1.1361165893462,-0.767317597823783,2.36536691413308));
#4073=CARTESIAN_POINT('Ctrl Pts',(-1.20297448753743,-0.647484519922585,
2.35526793587841));
#4074=CARTESIAN_POINT('Ctrl Pts',(-1.21264126062292,-0.629194013310627,
2.35376141243667));
#4075=CARTESIAN_POINT('Ctrl Pts',(-1.22587007589173,-0.602725340192119,
2.35163758550378));
#4076=CARTESIAN_POINT('Ctrl Pts',(-1.2297728455932,-0.594721815568319,2.35100260131887));
#4077=CARTESIAN_POINT('Ctrl Pts',(-1.23620947779529,-0.581187681579178,
2.34994159829172));
#4078=CARTESIAN_POINT('Ctrl Pts',(-1.23878506380021,-0.575677483767837,
2.3495131771138));
#4079=CARTESIAN_POINT('Ctrl Pts',(-1.24463829564584,-0.562933894261398,
2.34853061030841));
#4080=CARTESIAN_POINT('Ctrl Pts',(-1.24788979739124,-0.555688867819095,
2.3479780024788));
#4081=CARTESIAN_POINT('Ctrl Pts',(-1.25704957827883,-0.534793037739726,
2.34640021397833));
#4082=CARTESIAN_POINT('Ctrl Pts',(-1.26279852725655,-0.52107308495318,2.34538374334719));
#4083=CARTESIAN_POINT('Ctrl Pts',(-1.29228200719528,-0.447354544529492,
2.34001131754651));
#4084=CARTESIAN_POINT('Ctrl Pts',(-1.31196987232,-0.385818388774232,2.33583657202266));
#4085=CARTESIAN_POINT('Ctrl Pts',(-1.34259872947066,-0.260006441818594,
2.32750102290687));
#4086=CARTESIAN_POINT('Ctrl Pts',(-1.35344127489454,-0.195885179564962,
2.32334989436872));
#4087=CARTESIAN_POINT('Ctrl Pts',(-1.36388087542549,-0.0877259045414485,
2.31623926819673));
#4088=CARTESIAN_POINT('Ctrl Pts',(-1.36598924460494,-0.0440418313328702,
2.31333927938346));
#4089=CARTESIAN_POINT('Ctrl Pts',(-1.36600404927079,0.0163501997855103,
2.30924602844509));
#4090=CARTESIAN_POINT('Ctrl Pts',(-1.36570243894645,0.033033286908241,2.3081065629074));
#4091=CARTESIAN_POINT('Ctrl Pts',(-1.36465466392262,0.0618087103916622,
2.3061239323985));
#4092=CARTESIAN_POINT('Ctrl Pts',(-1.36405306326691,0.0739046187657651,
2.30528525914422));
#4093=CARTESIAN_POINT('Ctrl Pts',(-1.36248350611625,0.0987883005367717,
2.30354831021974));
#4094=CARTESIAN_POINT('Ctrl Pts',(-1.36149614205953,0.111573599444312,2.30264952065761));
#4095=CARTESIAN_POINT('Ctrl Pts',(-1.35846635477241,0.144719948123277,2.30030200332278));
#4096=CARTESIAN_POINT('Ctrl Pts',(-1.35614621387222,0.165051709732037,2.298844948199));
#4097=CARTESIAN_POINT('Ctrl Pts',(-1.34181863080126,0.269682828433087,2.29125401830345));
#4098=CARTESIAN_POINT('Ctrl Pts',(-1.32240649733088,0.352764312422965,2.28489767949591));
#4099=CARTESIAN_POINT('Ctrl Pts',(-1.26960619708709,0.510548536813381,2.27232432142413));
#4100=CARTESIAN_POINT('Ctrl Pts',(-1.23699115224955,0.585162017848858,2.26614210876987));
#4101=CARTESIAN_POINT('Ctrl Pts',(-1.19117302222158,0.668775569663828,2.25920115580365));
#4102=CARTESIAN_POINT('Ctrl Pts',(-1.18422164703187,0.681008855391917,2.25818561544659));
#4103=CARTESIAN_POINT('Ctrl Pts',(-1.17313969407658,0.699828283393194,2.25662572194617));
#4104=CARTESIAN_POINT('Ctrl Pts',(-1.16914003894161,0.70648987604062,2.25607403541721));
#4105=CARTESIAN_POINT('Ctrl Pts',(-1.16153149835778,0.718920632636567,2.25504597825618));
#4106=CARTESIAN_POINT('Ctrl Pts',(-1.15793618502672,0.724697241142232,2.25456887870297));
#4107=CARTESIAN_POINT('Ctrl Pts',(-1.15200861218155,0.734064357973069,2.25379598744767));
#4108=CARTESIAN_POINT('Ctrl Pts',(-1.14970257594817,0.737670869509345,2.25349858565013));
#4109=CARTESIAN_POINT('Ctrl Pts',(-1.14737960344529,0.741266514553124,2.25320219258599));
#4110=CARTESIAN_POINT('',(-1.36599953791183,0.00117996591060617,2.19095138131927));
#4111=CARTESIAN_POINT('Ctrl Pts',(-1.14737960371854,0.741266514130168,2.135049540568));
#4112=CARTESIAN_POINT('Ctrl Pts',(-1.17371791782586,0.700498391158188,2.13860808597731));
#4113=CARTESIAN_POINT('Ctrl Pts',(-1.19786310457235,0.658357968998659,2.1422315668744));
#4114=CARTESIAN_POINT('Ctrl Pts',(-1.25537449359362,0.544301663977534,2.15185451518902));
#4115=CARTESIAN_POINT('Ctrl Pts',(-1.2848175537371,0.470610192428532,2.15789704875815));
#4116=CARTESIAN_POINT('Ctrl Pts',(-1.31459053704653,0.37198739168062,2.16551368962053));
#4117=CARTESIAN_POINT('Ctrl Pts',(-1.32087503262053,0.349016059702377,2.16725510478538));
#4118=CARTESIAN_POINT('Ctrl Pts',(-1.32884726459755,0.316564638328336,2.16965941112887));
#4119=CARTESIAN_POINT('Ctrl Pts',(-1.3310400216991,0.307214415458845,2.17034573411801));
#4120=CARTESIAN_POINT('Ctrl Pts',(-1.33461520410095,0.291211953288213,2.17150852239933));
#4121=CARTESIAN_POINT('Ctrl Pts',(-1.33604691120638,0.28457126363952,2.1719875764289));
#4122=CARTESIAN_POINT('Ctrl Pts',(-1.33901597091823,0.270283301705197,2.17301060879284));
#4123=CARTESIAN_POINT('Ctrl Pts',(-1.34053745351382,0.262633160237652,2.17355373840162));
#4124=CARTESIAN_POINT('Ctrl Pts',(-1.34356997052004,0.246672007860385,2.17467809067034));
#4125=CARTESIAN_POINT('Ctrl Pts',(-1.34506961512004,0.238359149745227,2.17525871322365));
#4126=CARTESIAN_POINT('Ctrl Pts',(-1.34998212061336,0.209603886683836,2.17725173725914));
#4127=CARTESIAN_POINT('Ctrl Pts',(-1.3530069884155,0.189097085164622,2.17864622994722));
#4128=CARTESIAN_POINT('Ctrl Pts',(-1.36246580351747,0.113014678564882,2.18374728945422));
#4129=CARTESIAN_POINT('Ctrl Pts',(-1.36595118104071,0.0571264594019624,
2.18735323940492));
#4130=CARTESIAN_POINT('Ctrl Pts',(-1.3659994907434,0.00117952904397824,
2.19095149184204));
#4131=CARTESIAN_POINT('Ctrl Pts',(-1.36599949036158,0.00117997114881014,
2.19095146340787));
#4132=CARTESIAN_POINT('Ctrl Pts',(-1.36607646183637,-0.08792644085728,2.19668238319806));
#4133=CARTESIAN_POINT('Ctrl Pts',(-1.35743489945597,-0.176821291742645,
2.20238374650203));
#4134=CARTESIAN_POINT('Ctrl Pts',(-1.33687455700889,-0.28110092303994,2.20949613751109));
#4135=CARTESIAN_POINT('Ctrl Pts',(-1.33323261145016,-0.297896077059224,
2.21065444507774));
#4136=CARTESIAN_POINT('Ctrl Pts',(-1.32568879633879,-0.329769080175029,
2.21288030576275));
#4137=CARTESIAN_POINT('Ctrl Pts',(-1.32184400159832,-0.344857699669815,
2.21394599684218));
#4138=CARTESIAN_POINT('Ctrl Pts',(-1.31459400899412,-0.371404622689786,
2.21584399275958));
#4139=CARTESIAN_POINT('Ctrl Pts',(-1.31129470361084,-0.382890306403933,
2.21667287484779));
#4140=CARTESIAN_POINT('Ctrl Pts',(-1.30400968890188,-0.407051921202472,
2.21843361417204));
#4141=CARTESIAN_POINT('Ctrl Pts',(-1.29998888363092,-0.419715874918516,
2.21936651968309));
#4142=CARTESIAN_POINT('Ctrl Pts',(-1.28857731970357,-0.453919624669206,
2.22191454523546));
#4143=CARTESIAN_POINT('Ctrl Pts',(-1.28083192825725,-0.475335666865282,
2.2235408577773));
#4144=CARTESIAN_POINT('Ctrl Pts',(-1.2388896809886,-0.58282564361692,2.23186637088375));
#4145=CARTESIAN_POINT('Ctrl Pts',(-1.19654209088457,-0.665443522994749,
2.23882576515915));
#4146=CARTESIAN_POINT('Ctrl Pts',(-1.11901282319034,-0.785021644128266,
2.24960631527121));
#4147=CARTESIAN_POINT('Ctrl Pts',(-1.08957418588737,-0.825395199767631,
2.25338295966459));
#4148=CARTESIAN_POINT('Ctrl Pts',(-1.04039463163135,-0.88561208045601,2.25915435284955));
#4149=CARTESIAN_POINT('Ctrl Pts',(-1.02214392200986,-0.906615572066782,
2.26119583914786));
#4150=CARTESIAN_POINT('Ctrl Pts',(-0.996536920470781,-0.934327776795401,
2.26391332033117));
#4151=CARTESIAN_POINT('Ctrl Pts',(-0.98973143499818,-0.94153381762631,2.26462223904124));
#4152=CARTESIAN_POINT('Ctrl Pts',(-0.978098109267252,-0.953586317092375,
2.26581090723722));
#4153=CARTESIAN_POINT('Ctrl Pts',(-0.973311299893142,-0.958471646744947,
2.26629354565115));
#4154=CARTESIAN_POINT('Ctrl Pts',(-0.963090747458644,-0.968747015498945,
2.26731016472728));
#4155=CARTESIAN_POINT('Ctrl Pts',(-0.957648107806782,-0.974127649072518,
2.26784346609662));
#4156=CARTESIAN_POINT('Ctrl Pts',(-0.942189163193491,-0.989155682905238,
2.2693367029386));
#4157=CARTESIAN_POINT('Ctrl Pts',(-0.93207003498454,-0.998696586326021,
2.2702891341921));
#4158=CARTESIAN_POINT('Ctrl Pts',(-0.859168901304149,-1.06535857891352,
2.276990995642));
#4159=CARTESIAN_POINT('Ctrl Pts',(-0.791320699721666,-1.11668055654621,
2.28241036286789));
#4160=CARTESIAN_POINT('Ctrl Pts',(-0.671258474259176,-1.19102461038199,
2.29148951311705));
#4161=CARTESIAN_POINT('Ctrl Pts',(-0.621592482610981,-1.2176821327883,2.29511692499223));
#4162=CARTESIAN_POINT('Ctrl Pts',(-0.53730950319118,-1.25641665729695,2.30122765946126));
#4163=CARTESIAN_POINT('Ctrl Pts',(-0.503599929029577,-1.27030353564526,
2.30365994102189));
#4164=CARTESIAN_POINT('Ctrl Pts',(-0.454634103003027,-1.28821981992616,
2.3072021551681));
#4165=CARTESIAN_POINT('Ctrl Pts',(-0.439799234228894,-1.29335960639101,
2.30827639792034));
#4166=CARTESIAN_POINT('Ctrl Pts',(-0.4135074745571,-1.30196418724908,2.31018398347378));
#4167=CARTESIAN_POINT('Ctrl Pts',(-0.402087286265688,-1.30553627861508,
2.31101378107394));
#4168=CARTESIAN_POINT('Ctrl Pts',(-0.377953184439014,-1.31273842838228,
2.31277067601318));
#4169=CARTESIAN_POINT('Ctrl Pts',(-0.365230605971333,-1.3163348258283,2.31369875081637));
#4170=CARTESIAN_POINT('Ctrl Pts',(-0.330774218445289,-1.3255369283498,2.3162183490802));
#4171=CARTESIAN_POINT('Ctrl Pts',(-0.308951997726483,-1.33079235413189,
2.31782063931884));
#4172=CARTESIAN_POINT('Ctrl Pts',(-0.205421790578268,-1.35304182826893,
2.32545748847324));
#4173=CARTESIAN_POINT('Ctrl Pts',(-0.122409600565164,-1.36305984025793,
2.33169878629354));
#4174=CARTESIAN_POINT('Ctrl Pts',(0.0178985283095588,-1.36706894655092,
2.34230927371497));
#4175=CARTESIAN_POINT('Ctrl Pts',(0.0748605360730985,-1.36513523905382,
2.34662919684714));
#4176=CARTESIAN_POINT('Ctrl Pts',(0.161375927554686,-1.35676544997509,2.35309520711253));
#4177=CARTESIAN_POINT('Ctrl Pts',(0.191114013724558,-1.35289704298862,2.355299774167));
#4178=CARTESIAN_POINT('Ctrl Pts',(0.230734987908566,-1.34641030291933,2.35819357490472));
#4179=CARTESIAN_POINT('Ctrl Pts',(0.240748722971042,-1.34465586925658,2.35892118738686));
#4180=CARTESIAN_POINT('Ctrl Pts',(0.25750727920682,-1.34152650426607,2.36013155681761));
#4181=CARTESIAN_POINT('Ctrl Pts',(0.264262852953502,-1.34021211519801,2.36061745182815));
#4182=CARTESIAN_POINT('Ctrl Pts',(0.278406540718293,-1.33734915805822,2.36163017303405));
#4183=CARTESIAN_POINT('Ctrl Pts',(0.285792198632084,-1.33579032733665,2.36215644630473));
#4184=CARTESIAN_POINT('Ctrl Pts',(0.306253632952181,-1.33129422077803,2.36360830269464));
#4185=CARTESIAN_POINT('Ctrl Pts',(0.31930007208281,-1.32822554097555,2.36452703144254));
#4186=CARTESIAN_POINT('Ctrl Pts',(0.41970015891958,-1.30304530788675,2.37155798903011));
#4187=CARTESIAN_POINT('Ctrl Pts',(0.50472947988421,-1.27252816058713,2.37729238542969));
#4188=CARTESIAN_POINT('Ctrl Pts',(0.658573275720449,-1.19944464820414,2.38824774128926));
#4189=CARTESIAN_POINT('Ctrl Pts',(0.727825415521351,-1.15872956420119,2.39343552490092));
#4190=CARTESIAN_POINT('Ctrl Pts',(0.808776973810352,-1.10100245879927,2.40013916888293));
#4191=CARTESIAN_POINT('Ctrl Pts',(0.824212311974858,-1.08949557655875,2.40144823447628));
#4192=CARTESIAN_POINT('Ctrl Pts',(0.849322570160549,-1.06993710240308,2.40363307959904));
#4193=CARTESIAN_POINT('Ctrl Pts',(0.859138875451151,-1.06207090430935,2.40450168918216));
#4194=CARTESIAN_POINT('Ctrl Pts',(0.878187754022247,-1.04636937323252,2.40621689678582));
#4195=CARTESIAN_POINT('Ctrl Pts',(0.887427557938885,-1.03854461113943,2.40706302384555));
#4196=CARTESIAN_POINT('Ctrl Pts',(0.909689503117703,-1.01917798528235,2.40913728037559));
#4197=CARTESIAN_POINT('Ctrl Pts',(0.922597165485077,-1.00750840118373,2.41037051997282));
#4198=CARTESIAN_POINT('Ctrl Pts',(0.969252526263535,-0.963679648030682,
2.41494472308392));
#4199=CARTESIAN_POINT('Ctrl Pts',(1.00156742054044,-0.93004879390754,2.41834593192469));
#4200=CARTESIAN_POINT('Ctrl Pts',(1.10838421002038,-0.806847006720276,2.4304385193758));
#4201=CARTESIAN_POINT('Ctrl Pts',(1.17309903152954,-0.709474019122929,2.43941664640074));
#4202=CARTESIAN_POINT('Ctrl Pts',(1.23383120310332,-0.586552282893262,2.44950681363341));
#4203=CARTESIAN_POINT('Ctrl Pts',(1.24256368728954,-0.567819172986419,2.45101188686558));
#4204=CARTESIAN_POINT('Ctrl Pts',(1.25444423115412,-0.540744734715356,2.45313396511914));
#4205=CARTESIAN_POINT('Ctrl Pts',(1.25794059457768,-0.532560483598315,2.4537686166332));
#4206=CARTESIAN_POINT('Ctrl Pts',(1.26369079536452,-0.518727813279361,2.45482915093959));
#4207=CARTESIAN_POINT('Ctrl Pts',(1.26598726494741,-0.513097671931915,2.45525743281715));
#4208=CARTESIAN_POINT('Ctrl Pts',(1.27119567206641,-0.500080594415097,2.45623977733098));
#4209=CARTESIAN_POINT('Ctrl Pts',(1.27408091214045,-0.492683341367778,2.45679230186873));
#4210=CARTESIAN_POINT('Ctrl Pts',(1.28218562186744,-0.471356850874166,2.45837003997861));
#4211=CARTESIAN_POINT('Ctrl Pts',(1.28724247339092,-0.4573664934488,2.45938654179684));
#4212=CARTESIAN_POINT('Ctrl Pts',(1.31295533045673,-0.382421445280935,2.46474795759204));
#4213=CARTESIAN_POINT('Ctrl Pts',(1.3295149713477,-0.320140111734791,2.46891263054978));
#4214=CARTESIAN_POINT('Ctrl Pts',(1.35456290222315,-0.189339644744835,2.47748605796773));
#4215=CARTESIAN_POINT('Ctrl Pts',(1.36237903849839,-0.120884203031925,2.48188165161043));
#4216=CARTESIAN_POINT('Ctrl Pts',(1.36656615806065,-0.0112521408170147,
2.48907847432982));
#4217=CARTESIAN_POINT('Ctrl Pts',(1.36629008634054,0.0296747307462688,2.49179855063476));
#4218=CARTESIAN_POINT('Ctrl Pts',(1.36333532645016,0.0868293488464395,2.49568072268751));
#4219=CARTESIAN_POINT('Ctrl Pts',(1.36220021545034,0.103116841317082,2.49679644714451));
#4220=CARTESIAN_POINT('Ctrl Pts',(1.35972022305621,0.131385577778616,2.49875134257828));
#4221=CARTESIAN_POINT('Ctrl Pts',(1.35850812391533,0.143376832665842,2.49958636799586));
#4222=CARTESIAN_POINT('Ctrl Pts',(1.35566514611722,0.168213061224002,2.50132865344911));
#4223=CARTESIAN_POINT('Ctrl Pts',(1.35400999216437,0.181053978328443,2.50223658159003));
#4224=CARTESIAN_POINT('Ctrl Pts',(1.34917983277572,0.214742745771451,2.50463826111263));
#4225=CARTESIAN_POINT('Ctrl Pts',(1.34570426053134,0.235543252117025,2.50614108493688));
#4226=CARTESIAN_POINT('Ctrl Pts',(1.3224161729163,0.357479942047706,2.51507380921219));
#4227=CARTESIAN_POINT('Ctrl Pts',(1.2916934761076,0.456176611211052,2.52284148514849));
#4228=CARTESIAN_POINT('Ctrl Pts',(1.23209423391968,0.591535194512689,2.53402603477027));
#4229=CARTESIAN_POINT('Ctrl Pts',(1.21199522473418,0.631694612871495,2.53741189842259));
#4230=CARTESIAN_POINT('Ctrl Pts',(1.17714155224769,0.69352331364702,2.54267089216371));
#4231=CARTESIAN_POINT('Ctrl Pts',(1.16367880105885,0.715883144678285,2.54458263813417));
#4232=CARTESIAN_POINT('Ctrl Pts',(1.14434749565081,0.746001842165404,2.54715838784733));
#4233=CARTESIAN_POINT('Ctrl Pts',(1.13902537654685,0.754102874157724,2.54785124156434));
#4234=CARTESIAN_POINT('Ctrl Pts',(1.12982011718613,0.76779477740346,2.54902146450636));
#4235=CARTESIAN_POINT('Ctrl Pts',(1.12598068058318,0.773414399119225,2.5495015091841));
#4236=CARTESIAN_POINT('Ctrl Pts',(1.11767678546578,0.785375540075554,2.55052247273197));
#4237=CARTESIAN_POINT('Ctrl Pts',(1.11320010449364,0.791708071533136,2.55106259395232));
#4238=CARTESIAN_POINT('Ctrl Pts',(1.10048795402133,0.809369141217755,2.55256888136645));
#4239=CARTESIAN_POINT('Ctrl Pts',(1.0921315844605,0.820610007194054,2.55352750647935));
#4240=CARTESIAN_POINT('Ctrl Pts',(1.03329335926526,0.897267094340546,2.56007947175965));
#4241=CARTESIAN_POINT('Ctrl Pts',(0.977133054033637,0.958122092464455,2.56536239615268));
#4242=CARTESIAN_POINT('Ctrl Pts',(0.873161913583961,1.05206847222157,2.57437063874636));
#4243=CARTESIAN_POINT('Ctrl Pts',(0.828126524603272,1.08787208716941,2.57806983397526));
#4244=CARTESIAN_POINT('Ctrl Pts',(0.750697400048299,1.14182795161101,2.58428421288578));
#4245=CARTESIAN_POINT('Ctrl Pts',(0.719582273859238,1.16168784055319,2.58674586518172));
#4246=CARTESIAN_POINT('Ctrl Pts',(0.674080489329991,1.18820035519313,2.59032292805261));
#4247=CARTESIAN_POINT('Ctrl Pts',(0.660321668396492,1.19590127092951,2.59140162518712));
#4248=CARTESIAN_POINT('Ctrl Pts',(0.63588464373612,1.20902857671307,2.59331423046945));
#4249=CARTESIAN_POINT('Ctrl Pts',(0.625262434861344,1.2145559892951,2.59414452948381));
#4250=CARTESIAN_POINT('Ctrl Pts',(0.60279134771834,1.22587622286607,2.59589954688453));
#4251=CARTESIAN_POINT('Ctrl Pts',(0.590928547386279,1.23163848306527,2.59682520691561));
#4252=CARTESIAN_POINT('Ctrl Pts',(0.558804217754113,1.24667167942333,2.59933062356771));
#4253=CARTESIAN_POINT('Ctrl Pts',(0.538396981711344,1.25561977408922,2.60092093713052));
#4254=CARTESIAN_POINT('Ctrl Pts',(0.434127480452693,1.29833023665962,2.60904489385575));
#4255=CARTESIAN_POINT('Ctrl Pts',(0.347292113586577,1.32420210682373,2.61582661269119));
#4256=CARTESIAN_POINT('Ctrl Pts',(0.185721712651223,1.35534685734947,2.6282727065431));
#4257=CARTESIAN_POINT('Ctrl Pts',(0.111860261402536,1.3634320367304,2.63389294550674));
#4258=CARTESIAN_POINT('Ctrl Pts',(0.0244083580187489,1.36584665622211,2.64024919808147));
#4259=CARTESIAN_POINT('Ctrl Pts',(0.0111094020576111,1.36601957194127,2.64120748227421));
#4260=CARTESIAN_POINT('Ctrl Pts',(-0.00971714452040687,1.36598617363267,
2.64269307007227));
#4261=CARTESIAN_POINT('Ctrl Pts',(-0.0172437213387161,1.3659118970302,2.6432268600547));
#4262=CARTESIAN_POINT('Ctrl Pts',(-0.0315809791105177,1.3656518783728,2.64423730383272));
#4263=CARTESIAN_POINT('Ctrl Pts',(-0.0383914374033142,1.3654773930208,2.64471449440175));
#4264=CARTESIAN_POINT('Ctrl Pts',(-0.0553504021755864,1.36491591963152,
2.64589636959368));
#4265=CARTESIAN_POINT('Ctrl Pts',(-0.0654966887571556,1.36446668486708,
2.64659778472214));
#4266=CARTESIAN_POINT('Ctrl Pts',(-0.103249304131287,1.36237305574665,2.64918961210104));
#4267=CARTESIAN_POINT('Ctrl Pts',(-0.130810550317792,1.36000353022628,2.65104590518989));
#4268=CARTESIAN_POINT('Ctrl Pts',(-0.234006464636342,1.34796478700161,2.65792448349459));
#4269=CARTESIAN_POINT('Ctrl Pts',(-0.30886287185463,1.33280662544063,2.66277439570784));
#4270=CARTESIAN_POINT('Ctrl Pts',(-0.452350479051149,1.29100500999837,2.67240112038397));
#4271=CARTESIAN_POINT('Ctrl Pts',(-0.520865352393476,1.26491592751046,2.6771586256277));
#4272=CARTESIAN_POINT('Ctrl Pts',(-0.60412243008238,1.2252973177307,2.68337806233754));
#4273=CARTESIAN_POINT('Ctrl Pts',(-0.621115991490716,1.21677125768185,2.68467128740375));
#4274=CARTESIAN_POINT('Ctrl Pts',(-0.649006816212435,1.20204126407364,2.68683697369529));
#4275=CARTESIAN_POINT('Ctrl Pts',(-0.660006815532055,1.19603680272708,2.68770252971901));
#4276=CARTESIAN_POINT('Ctrl Pts',(-0.681498264492303,1.18391871623988,2.68941715435755));
#4277=CARTESIAN_POINT('Ctrl Pts',(-0.691993903453373,1.17781485470824,2.69026581910582));
#4278=CARTESIAN_POINT('Ctrl Pts',(-0.71749363730311,1.16252669694836,2.69235636132904));
#4279=CARTESIAN_POINT('Ctrl Pts',(-0.732403991128427,1.15319113042094,2.69360354224826));
#4280=CARTESIAN_POINT('Ctrl Pts',(-0.787347214267139,1.11729505879172,2.69829516395191));
#4281=CARTESIAN_POINT('Ctrl Pts',(-0.826146428853504,1.08891919775506,2.70180394607588));
#4282=CARTESIAN_POINT('Ctrl Pts',(-0.935272628256078,0.999915459480922,
2.71225949054176));
#4283=CARTESIAN_POINT('Ctrl Pts',(-1.00101373598797,0.934095958786727,2.71935360734661));
#4284=CARTESIAN_POINT('Ctrl Pts',(-1.08340050201359,0.832841597761097,2.72912570955183));
#4285=CARTESIAN_POINT('Ctrl Pts',(-1.10600946457868,0.802574216693599,2.7319206684085));
#4286=CARTESIAN_POINT('Ctrl Pts',(-1.13350576186215,0.762390985997101,2.73543780406233));
#4287=CARTESIAN_POINT('Ctrl Pts',(-1.13956648763224,0.753301777093282,2.73622113497334));
#4288=CARTESIAN_POINT('Ctrl Pts',(-1.14613957558168,0.743183272266232,2.73707895540836));
#4289=CARTESIAN_POINT('Ctrl Pts',(-1.14676018894998,0.742225283827124,2.73716003172249));
#4290=CARTESIAN_POINT('Ctrl Pts',(-1.1473796034465,0.741266514551254,2.73724103392041));
#4291=CARTESIAN_POINT('Origin',(0.,0.,-1.10921167016993));
#4292=CARTESIAN_POINT('',(-1.14737936922177,0.741266877099097,3.45490258866455));
#4293=CARTESIAN_POINT('',(-1.14737979714396,0.741266214733872,3.33530270583882));
#4294=CARTESIAN_POINT('',(-1.14737960344596,0.741266514552077,-1.10921167016993));
#4295=CARTESIAN_POINT('',(-1.3659998215671,-0.000698196705795024,2.90819715390762));
#4296=CARTESIAN_POINT('Ctrl Pts',(-1.14737936922177,0.741266877099097,3.45490258866455));
#4297=CARTESIAN_POINT('Ctrl Pts',(-1.11952596587337,0.784380121939649,3.45157440197762));
#4298=CARTESIAN_POINT('Ctrl Pts',(-1.08924219884794,0.825924191298115,3.44820368515017));
#4299=CARTESIAN_POINT('Ctrl Pts',(-1.04353816610939,0.881710130657872,3.44335396253766));
#4300=CARTESIAN_POINT('Ctrl Pts',(-1.03005527619933,0.897424487929018,3.44194906241363));
#4301=CARTESIAN_POINT('Ctrl Pts',(-1.00761943431487,0.922401627006729,3.43964762343261));
#4302=CARTESIAN_POINT('Ctrl Pts',(-0.998883160533326,0.931855191594713,
3.43875992684046));
#4303=CARTESIAN_POINT('Ctrl Pts',(-0.981685959800063,0.949944631053132,
3.43702769259532));
#4304=CARTESIAN_POINT('Ctrl Pts',(-0.973241389204758,0.95859444372604,3.43618389374785));
#4305=CARTESIAN_POINT('Ctrl Pts',(-0.952970205997118,0.978814328330803,
3.43417348411629));
#4306=CARTESIAN_POINT('Ctrl Pts',(-0.941046236186742,0.990283616741711,
3.43300270920174));
#4307=CARTESIAN_POINT('Ctrl Pts',(-0.897700566111386,1.03048652757841,3.4287861517702));
#4308=CARTESIAN_POINT('Ctrl Pts',(-0.865150400075602,1.05796167295573,3.42569059017237));
#4309=CARTESIAN_POINT('Ctrl Pts',(-0.776399187523272,1.12603756002686,3.4174289574481));
#4310=CARTESIAN_POINT('Ctrl Pts',(-0.718300540121299,1.16395837417859,3.41218970310328));
#4311=CARTESIAN_POINT('Ctrl Pts',(-0.603684223396136,1.22690775128098,3.40230006907409));
#4312=CARTESIAN_POINT('Ctrl Pts',(-0.547843889435548,1.25283904698977,3.39766236478986));
#4313=CARTESIAN_POINT('Ctrl Pts',(-0.476454819830723,1.28030128862273,3.39208379300223));
#4314=CARTESIAN_POINT('Ctrl Pts',(-0.462379542846903,1.28545158980115,3.39100037810259));
#4315=CARTESIAN_POINT('Ctrl Pts',(-0.440698293789413,1.29298277023957,3.38935947749768));
#4316=CARTESIAN_POINT('Ctrl Pts',(-0.433151983451155,1.29553031519802,3.38879347925848));
#4317=CARTESIAN_POINT('Ctrl Pts',(-0.419807567560481,1.29990559468693,3.38780213838708));
#4318=CARTESIAN_POINT('Ctrl Pts',(-0.41401914953979,1.30176076718246,3.38737531029461));
#4319=CARTESIAN_POINT('Ctrl Pts',(-0.399754189607378,1.30622787153547,3.38633104015039));
#4320=CARTESIAN_POINT('Ctrl Pts',(-0.39126428976378,1.30879598517655,3.38571604792524));
#4321=CARTESIAN_POINT('Ctrl Pts',(-0.363098380647745,1.31701732783122,3.38369538241295));
#4322=CARTESIAN_POINT('Ctrl Pts',(-0.343319331670952,1.32231124185327,3.38230789549032));
#4323=CARTESIAN_POINT('Ctrl Pts',(-0.19633467142663,1.35813128165645,3.37217749989463));
#4324=CARTESIAN_POINT('Ctrl Pts',(-0.0654425975497376,1.37069060462629,
3.36408625396289));
#4325=CARTESIAN_POINT('Ctrl Pts',(0.101041286051439,1.36272911653129,3.35310870086751));
#4326=CARTESIAN_POINT('Ctrl Pts',(0.136749279713942,1.3596099744566,3.35071857142971));
#4327=CARTESIAN_POINT('Ctrl Pts',(0.186641211857784,1.35326653324207,3.34730485105731));
#4328=CARTESIAN_POINT('Ctrl Pts',(0.200960869417467,1.35121425182602,3.34631648524208));
#4329=CARTESIAN_POINT('Ctrl Pts',(0.227162237245689,1.347033392174,3.34449073546578));
#4330=CARTESIAN_POINT('Ctrl Pts',(0.23905361500105,1.34497397545557,3.34365555244704));
#4331=CARTESIAN_POINT('Ctrl Pts',(0.263349696370282,1.34043386152849,3.34193485230474));
#4332=CARTESIAN_POINT('Ctrl Pts',(0.275750312982287,1.3379378705994,3.34104893384218));
#4333=CARTESIAN_POINT('Ctrl Pts',(0.307266506086722,1.33113755341733,3.33877687765412));
#4334=CARTESIAN_POINT('Ctrl Pts',(0.326326832066408,1.32659361526658,3.33738340755153));
#4335=CARTESIAN_POINT('Ctrl Pts',(0.430334887004992,1.29942126330434,3.32966858452517));
#4336=CARTESIAN_POINT('Ctrl Pts',(0.513029917941651,1.26904652813601,3.32310573772539));
#4337=CARTESIAN_POINT('Ctrl Pts',(0.664446318719396,1.19619858369405,3.31040605981962));
#4338=CARTESIAN_POINT('Ctrl Pts',(0.73347865816001,1.15515842671112,3.30431143572428));
#4339=CARTESIAN_POINT('Ctrl Pts',(0.809980461628674,1.10003966045376,3.29744639011927));
#4340=CARTESIAN_POINT('Ctrl Pts',(0.821314984340061,1.09160310494144,3.29642646717704));
#4341=CARTESIAN_POINT('Ctrl Pts',(0.838687172217952,1.07824876221461,3.29486132841733));
#4342=CARTESIAN_POINT('Ctrl Pts',(0.844816777322932,1.07345292695909,3.29430870521757));
#4343=CARTESIAN_POINT('Ctrl Pts',(0.856225282227469,1.06436859892801,3.29327995332105));
#4344=CARTESIAN_POINT('Ctrl Pts',(0.861513406191609,1.06009287399211,3.29280308154885));
#4345=CARTESIAN_POINT('Ctrl Pts',(0.874223891584747,1.04965785055443,3.29165639586456));
#4346=CARTESIAN_POINT('Ctrl Pts',(0.881613329402282,1.04345913520713,3.29098930470938));
#4347=CARTESIAN_POINT('Ctrl Pts',(0.908465109076654,1.0204453115064,3.28856091286791));
#4348=CARTESIAN_POINT('Ctrl Pts',(0.927518365159583,1.00315869654733,3.28682933073821));
#4349=CARTESIAN_POINT('Ctrl Pts',(0.977694467776746,0.954982299354946,3.28220909628167));
#4350=CARTESIAN_POINT('Ctrl Pts',(1.00783782006688,0.92311488980507,3.27936665356975));
#4351=CARTESIAN_POINT('Ctrl Pts',(1.1048713712067,0.810101160323626,3.2697648007979));
#4352=CARTESIAN_POINT('Ctrl Pts',(1.16390446942265,0.722723168632437,3.26308654107747));
#4353=CARTESIAN_POINT('Ctrl Pts',(1.22192481092492,0.610973728590381,3.25462072095394));
#4354=CARTESIAN_POINT('Ctrl Pts',(1.23109104241388,0.592287016308522,3.25320870657538));
#4355=CARTESIAN_POINT('Ctrl Pts',(1.24523875654687,0.561696258209988,3.25089859998073));
#4356=CARTESIAN_POINT('Ctrl Pts',(1.25048494755218,0.549917833617948,3.25000947942465));
#4357=CARTESIAN_POINT('Ctrl Pts',(1.26032130375748,0.52696499716382,3.2482765248527));
#4358=CARTESIAN_POINT('Ctrl Pts',(1.26493152895234,0.515800453191203,3.24743345619121));
#4359=CARTESIAN_POINT('Ctrl Pts',(1.275481594337,0.489259031831937,3.2454281471759));
#4360=CARTESIAN_POINT('Ctrl Pts',(1.28129222480163,0.473833188172663,3.24426180135614));
#4361=CARTESIAN_POINT('Ctrl Pts',(1.30094660852811,0.41864808440182,3.24008426157558));
#4362=CARTESIAN_POINT('Ctrl Pts',(1.313228810867,0.378361909673317,3.23702452433899));
#4363=CARTESIAN_POINT('Ctrl Pts',(1.34157596304562,0.267213311735129,3.22855580893986));
#4364=CARTESIAN_POINT('Ctrl Pts',(1.35388062846224,0.195536533686368,3.22305948959263));
#4365=CARTESIAN_POINT('Ctrl Pts',(1.36575687054721,0.0644244356058351,3.21310574377113));
#4366=CARTESIAN_POINT('Ctrl Pts',(1.3672655798415,0.00533101284859088,3.20865856982825));
#4367=CARTESIAN_POINT('Ctrl Pts',(1.36436194771161,-0.0685020762610586,
3.20327113986523));
#4368=CARTESIAN_POINT('Ctrl Pts',(1.3635375557866,-0.0833152919444829,3.20219896223031));
#4369=CARTESIAN_POINT('Ctrl Pts',(1.36190221834453,-0.106024864419903,3.20057143887855));
#4370=CARTESIAN_POINT('Ctrl Pts',(1.36126354269587,-0.113931995177353,3.20000778073755));
#4371=CARTESIAN_POINT('Ctrl Pts',(1.36001337906888,-0.127893012177758,3.19901842713312));
#4372=CARTESIAN_POINT('Ctrl Pts',(1.35943029989715,-0.133948780183741,3.19859127932164));
#4373=CARTESIAN_POINT('Ctrl Pts',(1.35789291934502,-0.148870143379656,3.19754348736508));
#4374=CARTESIAN_POINT('Ctrl Pts',(1.35689224499234,-0.157730613416601,3.19692533733126));
#4375=CARTESIAN_POINT('Ctrl Pts',(1.35327313049798,-0.18718664012045,3.19488189769329));
#4376=CARTESIAN_POINT('Ctrl Pts',(1.35027182307618,-0.20773329046104,3.19347536105528));
#4377=CARTESIAN_POINT('Ctrl Pts',(1.32728480686735,-0.343396431620855,3.1842661581634));
#4378=CARTESIAN_POINT('Ctrl Pts',(1.29306775888658,-0.455617894212942,3.17698369869951));
#4379=CARTESIAN_POINT('Ctrl Pts',(1.22598173093634,-0.604198678569807,3.16634275080618));
#4380=CARTESIAN_POINT('Ctrl Pts',(1.20486516005097,-0.645280201412293,3.16328820163393));
#4381=CARTESIAN_POINT('Ctrl Pts',(1.17300100941232,-0.700232926208892,3.15898916046204));
#4382=CARTESIAN_POINT('Ctrl Pts',(1.16400546042755,-0.715086541301879,3.15780476614719));
#4383=CARTESIAN_POINT('Ctrl Pts',(1.14826317073107,-0.739996079763346,3.15577765749067));
#4384=CARTESIAN_POINT('Ctrl Pts',(1.14166126251398,-0.75014135514566,3.15494020893623));
#4385=CARTESIAN_POINT('Ctrl Pts',(1.12791740261348,-0.770660052855567,3.15322132569112));
#4386=CARTESIAN_POINT('Ctrl Pts',(1.12076508546755,-0.781025088343883,3.15233956614868));
#4387=CARTESIAN_POINT('Ctrl Pts',(1.10228484173557,-0.807029743925583,3.15009205306045));
#4388=CARTESIAN_POINT('Ctrl Pts',(1.09076701920435,-0.822530316890012,3.14871928184725));
#4389=CARTESIAN_POINT('Ctrl Pts',(1.02835333040827,-0.90290896082275,3.14141976487176));
#4390=CARTESIAN_POINT('Ctrl Pts',(0.97199693635401,-0.963313519454494,3.13528262130146));
#4391=CARTESIAN_POINT('Ctrl Pts',(0.845616463623247,-1.07632551654564,3.12248340826263));
#4392=CARTESIAN_POINT('Ctrl Pts',(0.775274108763995,-1.12804963381647,3.11584084959659));
#4393=CARTESIAN_POINT('Ctrl Pts',(0.688671202598603,-1.17977845107784,3.10850449130767));
#4394=CARTESIAN_POINT('Ctrl Pts',(0.676755349651456,-1.18665388905116,3.10751247021067));
#4395=CARTESIAN_POINT('Ctrl Pts',(0.65807750653892,-1.19705810510458,3.10598659319119));
#4396=CARTESIAN_POINT('Ctrl Pts',(0.65138676501804,-1.20071203922276,3.10544569703378));
#4397=CARTESIAN_POINT('Ctrl Pts',(0.638623231183331,-1.20754434300906,3.10442512826929));
#4398=CARTESIAN_POINT('Ctrl Pts',(0.632556625004821,-1.21073328607801,3.10394487579284));
#4399=CARTESIAN_POINT('Ctrl Pts',(0.617589747883078,-1.21845749992736,3.10277135533876));
#4400=CARTESIAN_POINT('Ctrl Pts',(0.608663042524002,-1.22294116434434,3.10208113481952));
#4401=CARTESIAN_POINT('Ctrl Pts',(0.574130999300641,-1.23981396560229,3.09944512125668));
#4402=CARTESIAN_POINT('Ctrl Pts',(0.548188466376972,-1.25150099505823,3.09753607780207));
#4403=CARTESIAN_POINT('Ctrl Pts',(0.473959670343445,-1.28218918004764,3.09222045233245));
#4404=CARTESIAN_POINT('Ctrl Pts',(0.424928242181872,-1.29926269406566,3.08887863109367));
#4405=CARTESIAN_POINT('Ctrl Pts',(0.287750312819767,-1.33843070385525,3.07970452560338));
#4406=CARTESIAN_POINT('Ctrl Pts',(0.198201149326897,-1.35458892711181,3.07389272584933));
#4407=CARTESIAN_POINT('Ctrl Pts',(0.0855195448502148,-1.36350216601995,
3.06631124618276));
#4408=CARTESIAN_POINT('Ctrl Pts',(0.0632849461917286,-1.36471486865637,
3.06480354461368));
#4409=CARTESIAN_POINT('Ctrl Pts',(0.0278503386528507,-1.36577972677735,
3.06237670642066));
#4410=CARTESIAN_POINT('Ctrl Pts',(0.0146644093364811,-1.36598493320493,
3.06146835283433));
#4411=CARTESIAN_POINT('Ctrl Pts',(-0.0105006938828898,-1.36601216090849,
3.05972366376811));
#4412=CARTESIAN_POINT('Ctrl Pts',(-0.0224786525949524,-1.36586755669788,
3.05888843179733));
#4413=CARTESIAN_POINT('Ctrl Pts',(-0.0502284491741487,-1.36516743712146,
3.05694154201533));
#4414=CARTESIAN_POINT('Ctrl Pts',(-0.0659953691986541,-1.36449609845557,
3.05582644858491));
#4415=CARTESIAN_POINT('Ctrl Pts',(-0.118658299278119,-1.36133889317227,
3.05207045087925));
#4416=CARTESIAN_POINT('Ctrl Pts',(-0.155461625785447,-1.35762830206659,
3.04939328039257));
#4417=CARTESIAN_POINT('Ctrl Pts',(-0.249168995243895,-1.34432038473211,
3.04244015875177));
#4418=CARTESIAN_POINT('Ctrl Pts',(-0.305695718692348,-1.3326032753762,3.03811312551726));
#4419=CARTESIAN_POINT('Ctrl Pts',(-0.440674214949408,-1.29558290976022,
3.02753808668194));
#4420=CARTESIAN_POINT('Ctrl Pts',(-0.517916534412971,-1.26668595716403,
3.02127443261782));
#4421=CARTESIAN_POINT('Ctrl Pts',(-0.604730276651481,-1.22493018964236,
3.01426210347852));
#4422=CARTESIAN_POINT('Ctrl Pts',(-0.617274806783212,-1.2186568543032,3.01324986441966));
#4423=CARTESIAN_POINT('Ctrl Pts',(-0.636607407907734,-1.20861376257629,
3.01169392335762));
#4424=CARTESIAN_POINT('Ctrl Pts',(-0.64346332920066,-1.20497766385499,3.01114294351353));
#4425=CARTESIAN_POINT('Ctrl Pts',(-0.656274332310081,-1.19804271068511,
3.01011540607988));
#4426=CARTESIAN_POINT('Ctrl Pts',(-0.662236031260655,-1.19475762268562,
3.00963813027082));
#4427=CARTESIAN_POINT('Ctrl Pts',(-0.676624185980672,-1.1866884976963,3.00848799468822));
#4428=CARTESIAN_POINT('Ctrl Pts',(-0.685024726671796,-1.18185913594663,
3.00781790179144));
#4429=CARTESIAN_POINT('Ctrl Pts',(-0.71582422648948,-1.16371416260903,3.00536363552994));
#4430=CARTESIAN_POINT('Ctrl Pts',(-0.737893671034164,-1.14984699539792,
3.00361001357485));
#4431=CARTESIAN_POINT('Ctrl Pts',(-0.796769605218092,-1.11045892361194,
2.99890722233588));
#4432=CARTESIAN_POINT('Ctrl Pts',(-0.832740651735628,-1.08374552382827,
2.99600629735977));
#4433=CARTESIAN_POINT('Ctrl Pts',(-0.947096438791633,-0.989759125798017,
2.98646838246588));
#4434=CARTESIAN_POINT('Ctrl Pts',(-1.01915982252501,-0.91538286978294,2.97990266600291));
#4435=CARTESIAN_POINT('Ctrl Pts',(-1.09501017206169,-0.816916385130135,
2.97154936389669));
#4436=CARTESIAN_POINT('Ctrl Pts',(-1.10747571825278,-0.799935692344157,
2.97012080303913));
#4437=CARTESIAN_POINT('Ctrl Pts',(-1.12695990863045,-0.77206536143616,2.96779052875609));
#4438=CARTESIAN_POINT('Ctrl Pts',(-1.13422524723013,-0.761351841666792,
2.9668980907328));
#4439=CARTESIAN_POINT('Ctrl Pts',(-1.1479621778456,-0.740462175202806,2.96516336791937));
#4440=CARTESIAN_POINT('Ctrl Pts',(-1.15445344387798,-0.730300365731136,
2.96432190939742));
#4441=CARTESIAN_POINT('Ctrl Pts',(-1.16942615017782,-0.706162663715283,
2.9623280105459));
#4442=CARTESIAN_POINT('Ctrl Pts',(-1.17779273828415,-0.692118091694161,
2.96117159580155));
#4443=CARTESIAN_POINT('Ctrl Pts',(-1.206276986346,-0.642290312332412,2.95707991000993));
#4444=CARTESIAN_POINT('Ctrl Pts',(-1.22503027940676,-0.605756733735404,
2.95409875475125));
#4445=CARTESIAN_POINT('Ctrl Pts',(-1.27723982735175,-0.491672166178959,
2.94484482211019));
#4446=CARTESIAN_POINT('Ctrl Pts',(-1.30517592802723,-0.411820801235354,
2.93843026435818));
#4447=CARTESIAN_POINT('Ctrl Pts',(-1.3385806102332,-0.277603429747723,2.92799439333938));
#4448=CARTESIAN_POINT('Ctrl Pts',(-1.34849319317181,-0.224564073405041,
2.92395891538661));
#4449=CARTESIAN_POINT('Ctrl Pts',(-1.35675165708441,-0.159140176773375,
2.91918189821619));
#4450=CARTESIAN_POINT('Ctrl Pts',(-1.3581003123126,-0.147187709774169,2.91831736002777));
#4451=CARTESIAN_POINT('Ctrl Pts',(-1.36000948914384,-0.127995607518491,
2.91694386623046));
#4452=CARTESIAN_POINT('Ctrl Pts',(-1.36067043992439,-0.120766908941682,
2.91642987417944));
#4453=CARTESIAN_POINT('Ctrl Pts',(-1.36179481381425,-0.107285545018877,
2.91547791597109));
#4454=CARTESIAN_POINT('Ctrl Pts',(-1.36227286425605,-0.101034396492146,
2.91503917160784));
#4455=CARTESIAN_POINT('Ctrl Pts',(-1.36320052936008,-0.087696817401474,
2.91410832541328));
#4456=CARTESIAN_POINT('Ctrl Pts',(-1.36363796688507,-0.0806096504419577,
2.91361686864516));
#4457=CARTESIAN_POINT('Ctrl Pts',(-1.36458656073511,-0.0630101522076326,
2.91240357475843));
#4458=CARTESIAN_POINT('Ctrl Pts',(-1.36503153846035,-0.0524945305617169,
2.9116849495475));
#4459=CARTESIAN_POINT('Ctrl Pts',(-1.36577779296243,-0.0282201845049701,
2.91003846451426));
#4460=CARTESIAN_POINT('Ctrl Pts',(-1.36599278763656,-0.0144598598424152,
2.90911430339757));
#4461=CARTESIAN_POINT('Ctrl Pts',(-1.3659998215671,-0.000698196705795024,
2.90819715390762));
#4462=CARTESIAN_POINT('Ctrl Pts',(-1.36599982067117,-0.000699947383821987,
2.90819727058204));
#4463=CARTESIAN_POINT('Ctrl Pts',(-1.36603811834598,0.0740408376203964,
2.90321614895498));
#4464=CARTESIAN_POINT('Ctrl Pts',(-1.35994219632796,0.148668269478248,2.89844664933997));
#4465=CARTESIAN_POINT('Ctrl Pts',(-1.33468287822297,0.301721687836379,2.88846903957996));
#4466=CARTESIAN_POINT('Ctrl Pts',(-1.31462716037188,0.379694086415268,2.88327052164584));
#4467=CARTESIAN_POINT('Ctrl Pts',(-1.28141584216642,0.473603571526771,2.87655462545921));
#4468=CARTESIAN_POINT('Ctrl Pts',(-1.27461164296517,0.491621807866384,2.87524504963661));
#4469=CARTESIAN_POINT('Ctrl Pts',(-1.26273591880415,0.521164397471336,2.87305942050981));
#4470=CARTESIAN_POINT('Ctrl Pts',(-1.25788180213555,0.532773576182582,2.8721905437729));
#4471=CARTESIAN_POINT('Ctrl Pts',(-1.24804229519679,0.555421553639558,2.87047484834364));
#4472=CARTESIAN_POINT('Ctrl Pts',(-1.24306908319984,0.566464394811963,2.86962850142787));
#4473=CARTESIAN_POINT('Ctrl Pts',(-1.23059292474813,0.593211547522121,2.86755376085174));
#4474=CARTESIAN_POINT('Ctrl Pts',(-1.22293558005477,0.608841033446778,2.86632025539059));
#4475=CARTESIAN_POINT('Ctrl Pts',(-1.19438779833755,0.66439760440072,2.86185686834645));
#4476=CARTESIAN_POINT('Ctrl Pts',(-1.17182577137712,0.703427176205171,2.85857145578429));
#4477=CARTESIAN_POINT('Ctrl Pts',(-1.14737960323804,0.741266514873919,2.85523392653093));
#4478=CARTESIAN_POINT('Ctrl Pts',(-1.1473796034465,0.741266514551254,2.73724103392041));
#4479=CARTESIAN_POINT('Ctrl Pts',(-1.15057249896258,0.736324347167213,2.73765857589913));
#4480=CARTESIAN_POINT('Ctrl Pts',(-1.15373353944903,0.731361432152484,2.73807414686288));
#4481=CARTESIAN_POINT('Ctrl Pts',(-1.16026311675626,0.720962132331392,2.73893695727811));
#4482=CARTESIAN_POINT('Ctrl Pts',(-1.16362572187677,0.715522242863275,2.73938382129083));
#4483=CARTESIAN_POINT('Ctrl Pts',(-1.17280678645064,0.700433571122158,2.74061157363299));
#4484=CARTESIAN_POINT('Ctrl Pts',(-1.17854441742851,0.690735856122947,2.74138755581199));
#4485=CARTESIAN_POINT('Ctrl Pts',(-1.20330086510121,0.647685901691912,2.7447799985362));
#4486=CARTESIAN_POINT('Ctrl Pts',(-1.22103035859875,0.613608532537429,2.74732882893174));
#4487=CARTESIAN_POINT('Ctrl Pts',(-1.27685745433803,0.494272259371022,2.75594952402163));
#4488=CARTESIAN_POINT('Ctrl Pts',(-1.30764233936883,0.405885139262189,2.76183557573808));
#4489=CARTESIAN_POINT('Ctrl Pts',(-1.34008007110202,0.269031176714398,2.77101307531492));
#4490=CARTESIAN_POINT('Ctrl Pts',(-1.34858896758189,0.222484750179486,2.77414179489373));
#4491=CARTESIAN_POINT('Ctrl Pts',(-1.35686483943027,0.158638384962662,2.77850137814088));
#4492=CARTESIAN_POINT('Ctrl Pts',(-1.3587440561424,0.141643481867952,2.77966813280422));
#4493=CARTESIAN_POINT('Ctrl Pts',(-1.36141459506357,0.1124925369886,2.78168258205061));
#4494=CARTESIAN_POINT('Ctrl Pts',(-1.36236323578757,0.100352716433346,2.78252537308681));
#4495=CARTESIAN_POINT('Ctrl Pts',(-1.36387126562964,0.0770463730733692,
2.78415157395397));
#4496=CARTESIAN_POINT('Ctrl Pts',(-1.36445610548622,0.0658824399349569,
2.78493413232573));
#4497=CARTESIAN_POINT('Ctrl Pts',(-1.36564197883456,0.0362988520802211,
2.7870179949882));
#4498=CARTESIAN_POINT('Ctrl Pts',(-1.36600736889497,0.0178726187264417,
2.78832636254868));
#4499=CARTESIAN_POINT('Ctrl Pts',(-1.3659745287301,-0.063015633370386,2.79411859118324));
#4500=CARTESIAN_POINT('Ctrl Pts',(-1.36166519990677,-0.125392567677053,
2.79871756855995));
#4501=CARTESIAN_POINT('Ctrl Pts',(-1.34640244543437,-0.235685188781841,
2.80705880593072));
#4502=CARTESIAN_POINT('Ctrl Pts',(-1.33710375098041,-0.283725777890929,
2.8107632978638));
#4503=CARTESIAN_POINT('Ctrl Pts',(-1.31119822309319,-0.387394812160237,
2.81884133500443));
#4504=CARTESIAN_POINT('Ctrl Pts',(-1.29358040563398,-0.442680994410301,
2.8232043163905));
#4505=CARTESIAN_POINT('Ctrl Pts',(-1.26712512982714,-0.510459150288916,
2.82850871912857));
#4506=CARTESIAN_POINT('Ctrl Pts',(-1.26152512388556,-0.524146015205151,
2.82957734877268));
#4507=CARTESIAN_POINT('Ctrl Pts',(-1.25258546779407,-0.545021458220617,
2.83120055473033));
#4508=CARTESIAN_POINT('Ctrl Pts',(-1.24940386325231,-0.552275962268128,
2.83176338169252));
#4509=CARTESIAN_POINT('Ctrl Pts',(-1.24338855546033,-0.565673632377859,
2.83279993500512));
#4510=CARTESIAN_POINT('Ctrl Pts',(-1.2405721839201,-0.571823764171653,2.83327455847943));
#4511=CARTESIAN_POINT('Ctrl Pts',(-1.23374047548147,-0.586454144960777,
2.83440110910919));
#4512=CARTESIAN_POINT('Ctrl Pts',(-1.22968327380125,-0.594914349884119,
2.83505057069143));
#4513=CARTESIAN_POINT('Ctrl Pts',(-1.21501317789129,-0.624713472981697,
2.83733346368826));
#4514=CARTESIAN_POINT('Ctrl Pts',(-1.20392877965059,-0.64581700368879,2.83894162828406));
#4515=CARTESIAN_POINT('Ctrl Pts',(-1.17333534496054,-0.700535434287843,
2.84311698613099));
#4516=CARTESIAN_POINT('Ctrl Pts',(-1.1529339608084,-0.73362756498671,2.84564814583357));
#4517=CARTESIAN_POINT('Ctrl Pts',(-1.07471074880778,-0.849168516378234,
2.85466710124961));
#4518=CARTESIAN_POINT('Ctrl Pts',(-1.0092355419046,-0.926030734968269,2.86104017769009));
#4519=CARTESIAN_POINT('Ctrl Pts',(-0.916029546794738,-1.01370157143677,
2.86955628946027));
#4520=CARTESIAN_POINT('Ctrl Pts',(-0.895593024092759,-1.03180132756153,
2.87139288122427));
#4521=CARTESIAN_POINT('Ctrl Pts',(-0.863621214967416,-1.05845158846678,
2.87423108898476));
#4522=CARTESIAN_POINT('Ctrl Pts',(-0.852469948114355,-1.06745319769899,
2.87521479979023));
#4523=CARTESIAN_POINT('Ctrl Pts',(-0.831834799922186,-1.08358088259662,
2.87702529084324));
#4524=CARTESIAN_POINT('Ctrl Pts',(-0.822395670488086,-1.09076212308067,
2.87784981684258));
#4525=CARTESIAN_POINT('Ctrl Pts',(-0.801481092155196,-1.10624802056063,
2.87966955596181));
#4526=CARTESIAN_POINT('Ctrl Pts',(-0.789967688479182,-1.11449883286375,
2.88066669211616));
#4527=CARTESIAN_POINT('Ctrl Pts',(-0.755903603844608,-1.13811702415164,
2.88360469779057));
#4528=CARTESIAN_POINT('Ctrl Pts',(-0.733019426725775,-1.15298870429551,
2.88556332060396));
#4529=CARTESIAN_POINT('Ctrl Pts',(-0.678564999796174,-1.18610029787644,
2.89019217367044));
#4530=CARTESIAN_POINT('Ctrl Pts',(-0.646680362495519,-1.2037809217233,2.89287890613758));
#4531=CARTESIAN_POINT('Ctrl Pts',(-0.564956533945809,-1.24491389256219,
2.89969835570477));
#4532=CARTESIAN_POINT('Ctrl Pts',(-0.514334978053881,-1.26666705716267,
2.90386449078473));
#4533=CARTESIAN_POINT('Ctrl Pts',(-0.4048977017204,-1.30605017463155,2.91266055266583));
#4534=CARTESIAN_POINT('Ctrl Pts',(-0.345917798957106,-1.32289508640888,
2.91728041824287));
#4535=CARTESIAN_POINT('Ctrl Pts',(-0.271366749303691,-1.33885775432365,
2.92284067970463));
#4536=CARTESIAN_POINT('Ctrl Pts',(-0.256680592094837,-1.34175076627224,
2.92392264665069));
#4537=CARTESIAN_POINT('Ctrl Pts',(-0.234116020779326,-1.34581166345596,
2.9255617331797));
#4538=CARTESIAN_POINT('Ctrl Pts',(-0.226270501485679,-1.3471529285501,2.92612734041623));
#4539=CARTESIAN_POINT('Ctrl Pts',(-0.212414345430657,-1.34939730230734,
2.92711820123959));
#4540=CARTESIAN_POINT('Ctrl Pts',(-0.206408995988884,-1.35032894594766,
2.92754493626115));
#4541=CARTESIAN_POINT('Ctrl Pts',(-0.191622369869683,-1.35252192577307,
2.92858921803193));
#4542=CARTESIAN_POINT('Ctrl Pts',(-0.182834709098554,-1.35373785211867,
2.9292043124781));
#4543=CARTESIAN_POINT('Ctrl Pts',(-0.153712808649518,-1.35747861863225,
2.93122632690644));
#4544=CARTESIAN_POINT('Ctrl Pts',(-0.13333260208096,-1.35963169758096,2.93261502340063));
#4545=CARTESIAN_POINT('Ctrl Pts',(0.0175150984547588,-1.37214323300134,
2.94275041707114));
#4546=CARTESIAN_POINT('Ctrl Pts',(0.148827953610968,-1.3641633544585,2.95084519227101));
#4547=CARTESIAN_POINT('Ctrl Pts',(0.31204062511948,-1.33036325500022,2.96182354270446));
#4548=CARTESIAN_POINT('Ctrl Pts',(0.346769730847836,-1.32173603977694,2.96420984717898));
#4549=CARTESIAN_POINT('Ctrl Pts',(0.394998533707071,-1.30772362809998,2.96761887308816));
#4550=CARTESIAN_POINT('Ctrl Pts',(0.408813589097488,-1.30347088650567,2.9686064966643));
#4551=CARTESIAN_POINT('Ctrl Pts',(0.434029661415569,-1.29526822475088,2.9704311624269));
#4552=CARTESIAN_POINT('Ctrl Pts',(0.44545092535273,-1.29138490698756,2.97126601046926));
#4553=CARTESIAN_POINT('Ctrl Pts',(0.468738901745412,-1.28312112388687,2.97298631726014));
#4554=CARTESIAN_POINT('Ctrl Pts',(0.480599161747456,-1.27872608610648,2.97387218068276));
#4555=CARTESIAN_POINT('Ctrl Pts',(0.510679213563483,-1.26710178097673,2.97614471684802));
#4556=CARTESIAN_POINT('Ctrl Pts',(0.52880701281505,-1.2596440986052,2.97753873231356));
#4557=CARTESIAN_POINT('Ctrl Pts',(0.627854233867203,-1.21638174868616,2.98529561246204));
#4558=CARTESIAN_POINT('Ctrl Pts',(0.705294364260077,-1.17317531635511,2.99190346626583));
#4559=CARTESIAN_POINT('Ctrl Pts',(0.84329641083693,-1.0775516623371,3.00459406735545));
#4560=CARTESIAN_POINT('Ctrl Pts',(0.904525071478661,-1.02669506984421,3.01063288450529));
#4561=CARTESIAN_POINT('Ctrl Pts',(0.971078448516087,-0.960814325811905,
3.01745201832386));
#4562=CARTESIAN_POINT('Ctrl Pts',(0.981011492183948,-0.950670297217601,
3.01847695239219));
#4563=CARTESIAN_POINT('Ctrl Pts',(0.996151718747177,-0.934718420631223,
3.0200479962254));
#4564=CARTESIAN_POINT('Ctrl Pts',(1.0014700375319,-0.929018053739657,3.0206015993165));
#4565=CARTESIAN_POINT('Ctrl Pts',(1.0113316910845,-0.918264871241324,3.02163090804709));
#4566=CARTESIAN_POINT('Ctrl Pts',(1.01588635868133,-0.913223451104482,3.02210737355179));
#4567=CARTESIAN_POINT('Ctrl Pts',(1.02679301870335,-0.900968626094434,3.02325135913853));
#4568=CARTESIAN_POINT('Ctrl Pts',(1.03310681882641,-0.893721815111771,3.02391618846292));
#4569=CARTESIAN_POINT('Ctrl Pts',(1.05587779426728,-0.867022085361121,3.02632608500185));
#4570=CARTESIAN_POINT('Ctrl Pts',(1.07186735888629,-0.847175172507116,3.02804201635865));
#4571=CARTESIAN_POINT('Ctrl Pts',(1.11343370739737,-0.792518859752084,3.03260443673468));
#4572=CARTESIAN_POINT('Ctrl Pts',(1.13793113154398,-0.756924035589029,3.03540610824553));
#4573=CARTESIAN_POINT('Ctrl Pts',(1.21682910194141,-0.629773630375466,3.04505501390468));
#4574=CARTESIAN_POINT('Ctrl Pts',(1.26218515869129,-0.533079991672298,3.05181367991454));
#4575=CARTESIAN_POINT('Ctrl Pts',(1.30237933359725,-0.412540193491741,3.06035963767341));
#4576=CARTESIAN_POINT('Ctrl Pts',(1.30845900324475,-0.392831137265044,3.06175924281031));
#4577=CARTESIAN_POINT('Ctrl Pts',(1.31759959786085,-0.36062793598177,3.0640540693177));
#4578=CARTESIAN_POINT('Ctrl Pts',(1.3209344631474,-0.348214493133696,3.06494054230761));
#4579=CARTESIAN_POINT('Ctrl Pts',(1.3270656085596,-0.324035608728886,3.06667181060787));
#4580=CARTESIAN_POINT('Ctrl Pts',(1.32988180854566,-0.312276422259023,3.06751588589142));
#4581=CARTESIAN_POINT('Ctrl Pts',(1.33618892316195,-0.284306362902053,3.06952927688713));
#4582=CARTESIAN_POINT('Ctrl Pts',(1.33954141633956,-0.268066591267152,3.07070279522731));
#4583=CARTESIAN_POINT('Ctrl Pts',(1.35050381205793,-0.209608244295557,3.07494525000009));
#4584=CARTESIAN_POINT('Ctrl Pts',(1.35641903399939,-0.167101401659893,3.078064804932));
#4585=CARTESIAN_POINT('Ctrl Pts',(1.36672588145937,-0.0543865423439802,
3.08642721913703));
#4586=CARTESIAN_POINT('Ctrl Pts',(1.36771338807098,0.0160018991397118,3.09174584904177));
#4587=CARTESIAN_POINT('Ctrl Pts',(1.35948339321396,0.146242111334113,3.10161413065164));
#4588=CARTESIAN_POINT('Ctrl Pts',(1.35171610898976,0.206025975189913,3.1061523014105));
#4589=CARTESIAN_POINT('Ctrl Pts',(1.33713707255443,0.279718259830903,3.11163009487079));
#4590=CARTESIAN_POINT('Ctrl Pts',(1.33400741289273,0.294282387568384,3.11270674781424));
#4591=CARTESIAN_POINT('Ctrl Pts',(1.32884422774793,0.316531394697004,3.11433950934974));
#4592=CARTESIAN_POINT('Ctrl Pts',(1.32698093367108,0.324254090403611,3.11490401083776));
#4593=CARTESIAN_POINT('Ctrl Pts',(1.32357282599314,0.337857866811323,3.11589393031033));
#4594=CARTESIAN_POINT('Ctrl Pts',(1.32205602872183,0.343745287991373,3.11632081409706));
#4595=CARTESIAN_POINT('Ctrl Pts',(1.31822376260552,0.358219480599451,3.11736674976889));
#4596=CARTESIAN_POINT('Ctrl Pts',(1.31586367027127,0.366794079412151,3.11798332854142));
#4597=CARTESIAN_POINT('Ctrl Pts',(1.3077525433972,0.395176785611726,3.12001602859977));
#4598=CARTESIAN_POINT('Ctrl Pts',(1.30163636083861,0.414878658174687,3.12141366138616));
#4599=CARTESIAN_POINT('Ctrl Pts',(1.25324121162077,0.559147174512248,3.13160051610739));
#4600=CARTESIAN_POINT('Ctrl Pts',(1.19361024750254,0.677171541597833,3.13973389522076));
#4601=CARTESIAN_POINT('Ctrl Pts',(1.0976971803934,0.813798084122,3.15073596507826));
#4602=CARTESIAN_POINT('Ctrl Pts',(1.07626515710295,0.841937887114607,3.15309618846417));
#4603=CARTESIAN_POINT('Ctrl Pts',(1.04377119156495,0.88133107610186,3.15656382151183));
#4604=CARTESIAN_POINT('Ctrl Pts',(1.03356744969989,0.89327546634832,3.15763822013523));
#4605=CARTESIAN_POINT('Ctrl Pts',(1.01520768007995,0.914031422738658,3.15954817729045));
#4606=CARTESIAN_POINT('Ctrl Pts',(1.00713709203345,0.922916538657451,3.16038021350373));
#4607=CARTESIAN_POINT('Ctrl Pts',(0.990024454408335,0.94126449706572,3.16212967074029));
#4608=CARTESIAN_POINT('Ctrl Pts',(0.980961434869913,0.950706009220624,3.16304792153868));
#4609=CARTESIAN_POINT('Ctrl Pts',(0.956456834724979,0.975510501706488,3.1655099232792));
#4610=CARTESIAN_POINT('Ctrl Pts',(0.940781651515177,0.990636261914579,3.16706359918743));
#4611=CARTESIAN_POINT('Ctrl Pts',(0.875437028320698,1.05074048906373,3.17345955134833));
#4612=CARTESIAN_POINT('Ctrl Pts',(0.822857985305066,1.09240470288447,3.17842876831727));
#4613=CARTESIAN_POINT('Ctrl Pts',(0.705343641828679,1.17221204938615,3.18912003054992));
#4614=CARTESIAN_POINT('Ctrl Pts',(0.63987476205376,1.20919448707235,3.19484396343836));
#4615=CARTESIAN_POINT('Ctrl Pts',(0.545242003403673,1.25280315506044,3.20259259402316));
#4616=CARTESIAN_POINT('Ctrl Pts',(0.518399995913137,1.26414647351902,3.20473453284266));
#4617=CARTESIAN_POINT('Ctrl Pts',(0.48156244253946,1.27834290974406,3.20758154611282));
#4618=CARTESIAN_POINT('Ctrl Pts',(0.471868859243252,1.28195272038424,3.20832220613323));
#4619=CARTESIAN_POINT('Ctrl Pts',(0.455693228407617,1.28776804549336,3.20954299682627));
#4620=CARTESIAN_POINT('Ctrl Pts',(0.449234052998387,1.29003551552824,3.21002649461239));
#4621=CARTESIAN_POINT('Ctrl Pts',(0.435702735611525,1.29467167378254,3.21103072984589));
#4622=CARTESIAN_POINT('Ctrl Pts',(0.428627797448005,1.29703116179964,3.21155095906299));
#4623=CARTESIAN_POINT('Ctrl Pts',(0.409195801019743,1.30333535254139,3.21296750886231));
#4624=CARTESIAN_POINT('Ctrl Pts',(0.396800970735034,1.30716229490686,3.21385750935968));
#4625=CARTESIAN_POINT('Ctrl Pts',(0.316981576031758,1.33056672917876,3.21951361071622));
#4626=CARTESIAN_POINT('Ctrl Pts',(0.248178453989884,1.34510041011198,3.22404993716046));
#4627=CARTESIAN_POINT('Ctrl Pts',(0.0837636912153136,1.36677769667172,3.23472109346056));
#4628=CARTESIAN_POINT('Ctrl Pts',(-0.0120680235703268,1.3692880583612,3.24082597838604));
#4629=CARTESIAN_POINT('Ctrl Pts',(-0.12922758754514,1.36005030865457,3.24871295417904));
#4630=CARTESIAN_POINT('Ctrl Pts',(-0.151036884180881,1.35780130462963,3.25019811507849));
#4631=CARTESIAN_POINT('Ctrl Pts',(-0.18579211726466,1.35336961446285,3.25259727778144));
#4632=CARTESIAN_POINT('Ctrl Pts',(-0.198777602106361,1.35152338811212,3.25350093331701));
#4633=CARTESIAN_POINT('Ctrl Pts',(-0.223583558708352,1.34763135098632,3.25524213044176));
#4634=CARTESIAN_POINT('Ctrl Pts',(-0.235407659257654,1.34561624682529,3.25607864441217));
#4635=CARTESIAN_POINT('Ctrl Pts',(-0.262861939000636,1.3405644683166,3.2580369576039));
#4636=CARTESIAN_POINT('Ctrl Pts',(-0.278468324252178,1.33740975286302,3.25916232772686));
#4637=CARTESIAN_POINT('Ctrl Pts',(-0.33109248919721,1.32581116750349,3.26300009297437));
#4638=CARTESIAN_POINT('Ctrl Pts',(-0.367809283287446,1.31609776749508,3.26575099263491));
#4639=CARTESIAN_POINT('Ctrl Pts',(-0.461666145365464,1.28703366773176,3.27297632277202));
#4640=CARTESIAN_POINT('Ctrl Pts',(-0.518012192281605,1.26540642870932,3.27750746389944));
#4641=CARTESIAN_POINT('Ctrl Pts',(-0.643110514770034,1.2076311568008,3.2879249969103));
#4642=CARTESIAN_POINT('Ctrl Pts',(-0.710591852759295,1.16919854512066,3.29381331393724));
#4643=CARTESIAN_POINT('Ctrl Pts',(-0.786388251548101,1.1170315373354,3.30051754913645));
#4644=CARTESIAN_POINT('Ctrl Pts',(-0.798192944264324,1.10862708047793,3.3015641839305));
#4645=CARTESIAN_POINT('Ctrl Pts',(-0.816190485307102,1.09537703279293,3.30316115873663));
#4646=CARTESIAN_POINT('Ctrl Pts',(-0.822478602137293,1.0906634261262,3.30371936451729));
#4647=CARTESIAN_POINT('Ctrl Pts',(-0.834114353457998,1.08178333884228,3.30475221749119));
#4648=CARTESIAN_POINT('Ctrl Pts',(-0.839471933883153,1.07763111566948,3.30522769340953));
#4649=CARTESIAN_POINT('Ctrl Pts',(-0.852258654810983,1.0675679389301,3.30636266090605));
#4650=CARTESIAN_POINT('Ctrl Pts',(-0.859657448699566,1.06161914207697,3.30701957774967));
#4651=CARTESIAN_POINT('Ctrl Pts',(-0.886017679348187,1.0399686115815,3.30936319281732));
#4652=CARTESIAN_POINT('Ctrl Pts',(-0.904617026419111,1.02383116504975,3.3110228108336));
#4653=CARTESIAN_POINT('Ctrl Pts',(-0.952913445246717,0.979583140827175,
3.31538032904864));
#4654=CARTESIAN_POINT('Ctrl Pts',(-0.981802780023006,0.950626585495604,
3.31803818661512));
#4655=CARTESIAN_POINT('Ctrl Pts',(-1.06027487272279,0.864572112582399,3.32555670272216));
#4656=CARTESIAN_POINT('Ctrl Pts',(-1.10643401002204,0.804644752684246,3.33036227633641));
#4657=CARTESIAN_POINT('Ctrl Pts',(-1.14737979714392,0.741266214733938,3.33530270583882));
#4658=CARTESIAN_POINT('Origin',(0.,0.,-1.10921167016993));
#4659=CARTESIAN_POINT('',(-1.14737960320836,0.74126651491986,4.05331207395161));
#4660=CARTESIAN_POINT('',(-1.14737996054503,0.741265961811063,3.93545337707765));
#4661=CARTESIAN_POINT('',(-1.14737960344596,0.741266514552077,-1.10921167016993));
#4662=CARTESIAN_POINT('Ctrl Pts',(-1.14737960320835,0.741266514919876,4.0533120739516));
#4663=CARTESIAN_POINT('Ctrl Pts',(-1.14208271428851,0.749465377521597,4.05260232715036));
#4664=CARTESIAN_POINT('Ctrl Pts',(-1.13669776340969,0.757607746088199,4.05189678629783));
#4665=CARTESIAN_POINT('Ctrl Pts',(-1.12623276791154,0.773068621195708,4.05055677229775));
#4666=CARTESIAN_POINT('Ctrl Pts',(-1.12116768136847,0.780396297951655,4.04992153297595));
#4667=CARTESIAN_POINT('Ctrl Pts',(-1.11252365663574,0.792643748789292,4.04886024585331));
#4668=CARTESIAN_POINT('Ctrl Pts',(-1.10898301203017,0.797589921894349,4.04843179245646));
#4669=CARTESIAN_POINT('Ctrl Pts',(-1.10074545301862,0.808936627221012,4.04744935267161));
#4670=CARTESIAN_POINT('Ctrl Pts',(-1.09602561976999,0.815320101528871,4.04689690162227));
#4671=CARTESIAN_POINT('Ctrl Pts',(-1.08231009944922,0.83353569409133,4.04532002524266));
#4672=CARTESIAN_POINT('Ctrl Pts',(-1.0731762985526,0.845263025136454,4.04430429451972));
#4673=CARTESIAN_POINT('Ctrl Pts',(-1.02646981293868,0.903253824884703,4.03926567098439));
#4674=CARTESIAN_POINT('Ctrl Pts',(-0.986085436215801,0.947177293421521,
4.03539596949304));
#4675=CARTESIAN_POINT('Ctrl Pts',(-0.891756768900862,1.03717577497354,4.02699261472622));
#4676=CARTESIAN_POINT('Ctrl Pts',(-0.836840198185006,1.0819712594372,4.02247995630053));
#4677=CARTESIAN_POINT('Ctrl Pts',(-0.743334435194101,1.1468491245818,4.01502833824987));
#4678=CARTESIAN_POINT('Ctrl Pts',(-0.706830231939513,1.16970058840442,4.01217111700904));
#4679=CARTESIAN_POINT('Ctrl Pts',(-0.654837484535871,1.1989243193653,4.00812789062007));
#4680=CARTESIAN_POINT('Ctrl Pts',(-0.640217648957412,1.20679450470004,4.00699386359582));
#4681=CARTESIAN_POINT('Ctrl Pts',(-0.614703614391421,1.21993516911713,4.00501756884494));
#4682=CARTESIAN_POINT('Ctrl Pts',(-0.603875911347207,1.22533106455954,4.00417971366749));
#4683=CARTESIAN_POINT('Ctrl Pts',(-0.581401026284826,1.23616099315731,4.00244154325445));
#4684=CARTESIAN_POINT('Ctrl Pts',(-0.569746001559793,1.2415758648254,4.00154067930209));
#4685=CARTESIAN_POINT('Ctrl Pts',(-0.539212367616805,1.25524119221851,3.99918104018996));
#4686=CARTESIAN_POINT('Ctrl Pts',(-0.520221057498316,1.26323014434989,3.99771377386539));
#4687=CARTESIAN_POINT('Ctrl Pts',(-0.401854854599082,1.30990065568995,3.9885660718615));
#4688=CARTESIAN_POINT('Ctrl Pts',(-0.298429681328461,1.33725790159594,3.98051900895684));
#4689=CARTESIAN_POINT('Ctrl Pts',(-0.150236307247837,1.35839697366796,3.96920211135042));
#4690=CARTESIAN_POINT('Ctrl Pts',(-0.10730545511775,1.36246072458844,3.96595408418624));
#4691=CARTESIAN_POINT('Ctrl Pts',(-0.0388316021290574,1.3656850844737,3.9608785237859));
#4692=CARTESIAN_POINT('Ctrl Pts',(-0.0133804685179279,1.36617158561613,
3.95901515310712));
#4693=CARTESIAN_POINT('Ctrl Pts',(0.0216790831681687,1.36586175577261,3.9564924867223));
#4694=CARTESIAN_POINT('Ctrl Pts',(0.031286155222495,1.36567547704529,3.95580580095057));
#4695=CARTESIAN_POINT('Ctrl Pts',(0.0476829726300942,1.36518442306701,3.95464249476632));
#4696=CARTESIAN_POINT('Ctrl Pts',(0.0544737087200887,1.36493032723659,3.95416328198851));
#4697=CARTESIAN_POINT('Ctrl Pts',(0.0690557680303902,1.36427568891862,3.9531399970622));
#4698=CARTESIAN_POINT('Ctrl Pts',(0.0768459492642894,1.36385906974782,3.9525967730755));
#4699=CARTESIAN_POINT('Ctrl Pts',(0.0988194919360919,1.36249504875585,3.95107316458252));
#4700=CARTESIAN_POINT('Ctrl Pts',(0.112992696456738,1.36139294106664,3.95010059541585));
#4701=CARTESIAN_POINT('Ctrl Pts',(0.206076618152484,1.35269094425106,3.94376495437454));
#4702=CARTESIAN_POINT('Ctrl Pts',(0.284224704194373,1.33845428421515,3.9386853819621));
#4703=CARTESIAN_POINT('Ctrl Pts',(0.418027768507446,1.30182220376946,3.92976785574138));
#4704=CARTESIAN_POINT('Ctrl Pts',(0.474263493616308,1.28240470081501,3.9259480926769));
#4705=CARTESIAN_POINT('Ctrl Pts',(0.563762887828581,1.24480712250549,3.91956057669029));
#4706=CARTESIAN_POINT('Ctrl Pts',(0.597852180167037,1.22879849714789,3.91705067584516));
#4707=CARTESIAN_POINT('Ctrl Pts',(0.645315937264399,1.20406621876125,3.91341627069128));
#4708=CARTESIAN_POINT('Ctrl Pts',(0.659267630754048,1.19648413018064,3.91233019116378));
#4709=CARTESIAN_POINT('Ctrl Pts',(0.683518133697531,1.18275219471639,3.91040903882213));
#4710=CARTESIAN_POINT('Ctrl Pts',(0.693874193412884,1.17670658236707,3.90957767915763));
#4711=CARTESIAN_POINT('Ctrl Pts',(0.715409870394442,1.16375143936165,3.90782498122307));
#4712=CARTESIAN_POINT('Ctrl Pts',(0.726571998716415,1.15681537187092,3.90690275625596));
#4713=CARTESIAN_POINT('Ctrl Pts',(0.756180610067992,1.13781921000519,3.90441827227017));
#4714=CARTESIAN_POINT('Ctrl Pts',(0.774437519508722,1.12547238895604,3.90284576740652));
#4715=CARTESIAN_POINT('Ctrl Pts',(0.86919202278311,1.05799427049293,3.89446210697466));
#4716=CARTESIAN_POINT('Ctrl Pts',(0.940115451856715,0.995501844818055,3.88737737808013));
#4717=CARTESIAN_POINT('Ctrl Pts',(1.05234617737867,0.873842881775787,3.87485639201078));
#4718=CARTESIAN_POINT('Ctrl Pts',(1.09649570494904,0.817760932135827,3.86946611340806));
#4719=CARTESIAN_POINT('Ctrl Pts',(1.14329340629184,0.747666636609126,3.86334664153477));
#4720=CARTESIAN_POINT('Ctrl Pts',(1.15036175866152,0.73674491384644,3.86240979884508));
#4721=CARTESIAN_POINT('Ctrl Pts',(1.16124025729096,0.719397538031531,3.86094972245166));
#4722=CARTESIAN_POINT('Ctrl Pts',(1.16515537050219,0.713039074835206,3.86042034670374));
#4723=CARTESIAN_POINT('Ctrl Pts',(1.17255871320137,0.700791626263941,3.85941220200326));
#4724=CARTESIAN_POINT('Ctrl Pts',(1.17605511838829,0.694908051639531,3.85893296885762));
#4725=CARTESIAN_POINT('Ctrl Pts',(1.18471601775466,0.680081320179104,3.85773737078964));
#4726=CARTESIAN_POINT('Ctrl Pts',(1.18982372780428,0.671105176515035,3.85702444775258));
#4727=CARTESIAN_POINT('Ctrl Pts',(1.20887819267441,0.636717909648691,3.8543310925829));
#4728=CARTESIAN_POINT('Ctrl Pts',(1.22211765267857,0.61092135060804,3.85238832599843));
#4729=CARTESIAN_POINT('Ctrl Pts',(1.26670573313672,0.516782102638326,3.84550368836485));
#4730=CARTESIAN_POINT('Ctrl Pts',(1.29322326128214,0.446298428134795,3.84072116467038));
#4731=CARTESIAN_POINT('Ctrl Pts',(1.33216551338004,0.309495122593954,3.83155770492004));
#4732=CARTESIAN_POINT('Ctrl Pts',(1.34574835656394,0.243746039092624,3.82720187021231));
#4733=CARTESIAN_POINT('Ctrl Pts',(1.35727655445153,0.155663679178198,3.8212389552559));
#4734=CARTESIAN_POINT('Ctrl Pts',(1.35958683732327,0.13399392273707,3.81976250220164));
#4735=CARTESIAN_POINT('Ctrl Pts',(1.36245381306657,0.0992320132374689,3.81737380587953));
#4736=CARTESIAN_POINT('Ctrl Pts',(1.36334222009293,0.0861705038528794,3.81647173942253));
#4737=CARTESIAN_POINT('Ctrl Pts',(1.3646852321018,0.061109487253447,3.81473125139453));
#4738=CARTESIAN_POINT('Ctrl Pts',(1.36516961348148,0.0491127518764308,3.81389382642674));
#4739=CARTESIAN_POINT('Ctrl Pts',(1.3659226523147,0.0214051459700489,3.8119491641948));
#4740=CARTESIAN_POINT('Ctrl Pts',(1.36607848364207,0.00569318591026028,
3.81083858586827));
#4741=CARTESIAN_POINT('Ctrl Pts',(1.36570829514905,-0.0447853615416102,
3.80724383510106));
#4742=CARTESIAN_POINT('Ctrl Pts',(1.36412602245752,-0.0795279528043798,
3.80472851984214));
#4743=CARTESIAN_POINT('Ctrl Pts',(1.35220396878944,-0.221671866906366,3.7942647253221));
#4744=CARTESIAN_POINT('Ctrl Pts',(1.33048410786226,-0.327720530562291,3.78601210613619));
#4745=CARTESIAN_POINT('Ctrl Pts',(1.28398875824084,-0.467882817824271,3.77494227704189));
#4746=CARTESIAN_POINT('Ctrl Pts',(1.26980423902497,-0.505113120920413,3.77199031408476));
#4747=CARTESIAN_POINT('Ctrl Pts',(1.2496141265528,-0.551854625200745,3.76831076386427));
#4748=CARTESIAN_POINT('Ctrl Pts',(1.245092411278,-0.561982117374848,3.76751519229196));
#4749=CARTESIAN_POINT('Ctrl Pts',(1.23749092837609,-0.578465254763044,3.76622438433666));
#4750=CARTESIAN_POINT('Ctrl Pts',(1.23448441474231,-0.584853901383183,3.76572509068309));
#4751=CARTESIAN_POINT('Ctrl Pts',(1.22828628854823,-0.597763747123393,3.76471860349242));
#4752=CARTESIAN_POINT('Ctrl Pts',(1.22509197531668,-0.604283346014246,3.76421158099726));
#4753=CARTESIAN_POINT('Ctrl Pts',(1.21646542919891,-0.621540548594131,3.76287205557516));
#4754=CARTESIAN_POINT('Ctrl Pts',(1.21094289942153,-0.632232641821085,3.76204476736161));
#4755=CARTESIAN_POINT('Ctrl Pts',(1.18005482482532,-0.690144623905229,3.75757075799206));
#4756=CARTESIAN_POINT('Ctrl Pts',(1.15206524884962,-0.735918462828498,3.75405872010642));
#4757=CARTESIAN_POINT('Ctrl Pts',(1.07552641805855,-0.845972513716948,3.74537992768325));
#4758=CARTESIAN_POINT('Ctrl Pts',(1.02385599755088,-0.9078245429899,3.74027461564287));
#4759=CARTESIAN_POINT('Ctrl Pts',(0.935755798912973,-0.996132303607631,
3.73211587373916));
#4760=CARTESIAN_POINT('Ctrl Pts',(0.902963622464841,-1.02595057475716,3.72917832519551));
#4761=CARTESIAN_POINT('Ctrl Pts',(0.855852805372316,-1.06477826029701,3.72504118545221));
#4762=CARTESIAN_POINT('Ctrl Pts',(0.842727860078257,-1.07519601968212,3.72389701753201));
#4763=CARTESIAN_POINT('Ctrl Pts',(0.819783281569719,-1.09272975537118,3.72190889579552));
#4764=CARTESIAN_POINT('Ctrl Pts',(0.810054215651539,-1.09996140764752,3.72106950492588));
#4765=CARTESIAN_POINT('Ctrl Pts',(0.789857185221242,-1.11456065571255,3.71933355074658));
#4766=CARTESIAN_POINT('Ctrl Pts',(0.779379358715203,-1.12191248491214,3.71843650312691));
#4767=CARTESIAN_POINT('Ctrl Pts',(0.751983224858947,-1.14056615203839,3.7160991701994));
#4768=CARTESIAN_POINT('Ctrl Pts',(0.734913510345819,-1.15163881975122,3.7146506943042));
#4769=CARTESIAN_POINT('Ctrl Pts',(0.625347417565087,-1.21928339982075,3.70539712076858));
#4770=CARTESIAN_POINT('Ctrl Pts',(0.52665296724612,-1.26504528002418,3.69721042016922));
#4771=CARTESIAN_POINT('Ctrl Pts',(0.383456552088563,-1.31175500748649,3.68582538989112));
#4772=CARTESIAN_POINT('Ctrl Pts',(0.342711785579238,-1.3229849390831,3.68264363424592));
#4773=CARTESIAN_POINT('Ctrl Pts',(0.284602036170661,-1.33613554930096,3.67823387564487));
#4774=CARTESIAN_POINT('Ctrl Pts',(0.267621793092662,-1.33963993639185,3.67696053573363));
#4775=CARTESIAN_POINT('Ctrl Pts',(0.237340589885816,-1.34529059801129,3.67472165685656));
#4776=CARTESIAN_POINT('Ctrl Pts',(0.2240660780003,-1.34756512869085,3.67375098439123));
#4777=CARTESIAN_POINT('Ctrl Pts',(0.203287084045003,-1.3508099643597,3.67225053306896));
#4778=CARTESIAN_POINT('Ctrl Pts',(0.195804893242241,-1.35191480839153,3.67171406710795));
#4779=CARTESIAN_POINT('Ctrl Pts',(0.181578765653415,-1.35389489612398,3.67070179801365));
#4780=CARTESIAN_POINT('Ctrl Pts',(0.174836925363774,-1.35478200811832,3.67022541829852));
#4781=CARTESIAN_POINT('Ctrl Pts',(0.158093345505703,-1.35685811170385,3.6690500585778));
#4782=CARTESIAN_POINT('Ctrl Pts',(0.148084307728478,-1.35798692714812,3.66835426286463));
#4783=CARTESIAN_POINT('Ctrl Pts',(0.111189533953986,-1.36173512179498,3.66581148366647));
#4784=CARTESIAN_POINT('Ctrl Pts',(0.0842385544339021,-1.36366775507627,
3.66399696632538));
#4785=CARTESIAN_POINT('Ctrl Pts',(-0.019443266028587,-1.36801664787397,
3.65712067915906));
#4786=CARTESIAN_POINT('Ctrl Pts',(-0.0962727424055962,-1.36476404760319,
3.65223780242633));
#4787=CARTESIAN_POINT('Ctrl Pts',(-0.221135549751428,-1.34887583653217,
3.64413073758124));
#4788=CARTESIAN_POINT('Ctrl Pts',(-0.26947205565319,-1.34005644581843,3.64095052757975));
#4789=CARTESIAN_POINT('Ctrl Pts',(-0.339819345587557,-1.32326050189445,
3.63617065003189));
#4790=CARTESIAN_POINT('Ctrl Pts',(-0.362270082488954,-1.31729109870488,
3.63462218416654));
#4791=CARTESIAN_POINT('Ctrl Pts',(-0.4033346413958,-1.30524332028537,3.63173847237445));
#4792=CARTESIAN_POINT('Ctrl Pts',(-0.421991092386243,-1.29933152507113,
3.63040840594825));
#4793=CARTESIAN_POINT('Ctrl Pts',(-0.452482205282357,-1.28894365039595,
3.62819794925531));
#4794=CARTESIAN_POINT('Ctrl Pts',(-0.464393491762242,-1.28470017760663,
3.62732508311039));
#4795=CARTESIAN_POINT('Ctrl Pts',(-0.487557531635201,-1.27608360413919,
3.62560832775299));
#4796=CARTESIAN_POINT('Ctrl Pts',(-0.498814630864025,-1.27172546524865,
3.6247649946738));
#4797=CARTESIAN_POINT('Ctrl Pts',(-0.523443209477178,-1.26181330577374,
3.62289926627383));
#4798=CARTESIAN_POINT('Ctrl Pts',(-0.536786969811317,-1.25619478291802,
3.62187482287878));
#4799=CARTESIAN_POINT('Ctrl Pts',(-0.582914280927707,-1.23590327854429,
3.61828456741328));
#4800=CARTESIAN_POINT('Ctrl Pts',(-0.615204050231333,-1.22015144023272,
3.61568375923047));
#4801=CARTESIAN_POINT('Ctrl Pts',(-0.761996032589823,-1.1412334505094,3.60344290419936));
#4802=CARTESIAN_POINT('Ctrl Pts',(-0.867653545564788,-1.06311889650848,
3.59333082567513));
#4803=CARTESIAN_POINT('Ctrl Pts',(-0.975135212519098,-0.956810119947042,
3.58220864934236));
#4804=CARTESIAN_POINT('Ctrl Pts',(-0.989352285032393,-0.94210214585143,
3.58071942172653));
#4805=CARTESIAN_POINT('Ctrl Pts',(-1.00925185925515,-0.9205679189021,3.57861523452353));
#4806=CARTESIAN_POINT('Ctrl Pts',(-1.01520583026031,-0.913997670562352,
3.57798301730475));
#4807=CARTESIAN_POINT('Ctrl Pts',(-1.02513296918479,-0.902826305626476,
3.57692508918283));
#4808=CARTESIAN_POINT('Ctrl Pts',(-1.02914000414453,-0.898255976777378,
3.57649701131207));
#4809=CARTESIAN_POINT('Ctrl Pts',(-1.03832843977742,-0.887633660887679,
3.57551303732085));
#4810=CARTESIAN_POINT('Ctrl Pts',(-1.04348759392396,-0.881562881559416,
3.57495870596985));
#4811=CARTESIAN_POINT('Ctrl Pts',(-1.0582045244594,-0.863935228960948,3.5733708738656));
#4812=CARTESIAN_POINT('Ctrl Pts',(-1.0676258131772,-0.85226525467405,3.57234625392496));
#4813=CARTESIAN_POINT('Ctrl Pts',(-1.11474723850734,-0.791888838203964,
3.56716523136413));
#4814=CARTESIAN_POINT('Ctrl Pts',(-1.14931828578632,-0.740822855988824,
3.56317243354008));
#4815=CARTESIAN_POINT('Ctrl Pts',(-1.20839521058935,-0.639410895328169,
3.55561232545762));
#4816=CARTESIAN_POINT('Ctrl Pts',(-1.23348606879065,-0.589556823505201,
3.55204751233129));
#4817=CARTESIAN_POINT('Ctrl Pts',(-1.27643807509572,-0.489383012109559,
3.54496457633142));
#4818=CARTESIAN_POINT('Ctrl Pts',(-1.29453646541553,-0.439277009436666,
3.54145785384923));
#4819=CARTESIAN_POINT('Ctrl Pts',(-1.31469513353201,-0.371276192092175,
3.53666116900418));
#4820=CARTESIAN_POINT('Ctrl Pts',(-1.319395445904,-0.354210268267431,3.53545455005704));
#4821=CARTESIAN_POINT('Ctrl Pts',(-1.32679414353658,-0.325152640008996,
3.53339268606863));
#4822=CARTESIAN_POINT('Ctrl Pts',(-1.32966477699609,-0.313206804550987,
3.53254295312185));
#4823=CARTESIAN_POINT('Ctrl Pts',(-1.3351384253474,-0.288995782869566,3.53081574687679));
#4824=CARTESIAN_POINT('Ctrl Pts',(-1.33773447463021,-0.276730255366954,
3.52993814606494));
#4825=CARTESIAN_POINT('Ctrl Pts',(-1.34384418853653,-0.245765658863391,
3.52771529941282));
#4826=CARTESIAN_POINT('Ctrl Pts',(-1.34713659244508,-0.227026207366572,
3.52636334799685));
#4827=CARTESIAN_POINT('Ctrl Pts',(-1.36072517230166,-0.138923985954145,
3.51997258211696));
#4828=CARTESIAN_POINT('Ctrl Pts',(-1.36606043483702,-0.0689134526760029,
3.51478621825296));
#4829=CARTESIAN_POINT('Ctrl Pts',(-1.36591336273895,0.100237112258158,3.50206631011594));
#4830=CARTESIAN_POINT('Ctrl Pts',(-1.35505465627204,0.198985499722037,3.49447306626828));
#4831=CARTESIAN_POINT('Ctrl Pts',(-1.33054415173034,0.309530476555009,3.48622831422803));
#4832=CARTESIAN_POINT('Ctrl Pts',(-1.32726100393754,0.32331891812312,3.48520511786736));
#4833=CARTESIAN_POINT('Ctrl Pts',(-1.32184107198603,0.344605418343624,3.48363606264008));
#4834=CARTESIAN_POINT('Ctrl Pts',(-1.31985381764948,0.352140059614764,3.48308274092917));
#4835=CARTESIAN_POINT('Ctrl Pts',(-1.31601228328548,0.366215623071584,3.48205346665481));
#4836=CARTESIAN_POINT('Ctrl Pts',(-1.3141735713459,0.372760028651765,3.48157676048259));
#4837=CARTESIAN_POINT('Ctrl Pts',(-1.3096132146034,0.388538137378118,3.48043151329544));
#4838=CARTESIAN_POINT('Ctrl Pts',(-1.30684269579416,0.397757260168607,3.4797656766112));
#4839=CARTESIAN_POINT('Ctrl Pts',(-1.29635441351563,0.431364751593982,3.47734801008214));
#4840=CARTESIAN_POINT('Ctrl Pts',(-1.28804901717805,0.455565846818251,3.47562555715607));
#4841=CARTESIAN_POINT('Ctrl Pts',(-1.2638145937603,0.520208419083282,3.47103923109373));
#4842=CARTESIAN_POINT('Ctrl Pts',(-1.24662722097694,0.560147477642661,3.46822074503088));
#4843=CARTESIAN_POINT('Ctrl Pts',(-1.20366875163054,0.648155048570496,3.4619067818998));
#4844=CARTESIAN_POINT('Ctrl Pts',(-1.17688798654137,0.69559158824865,3.45842855588962));
#4845=CARTESIAN_POINT('Ctrl Pts',(-1.14737936922177,0.741266877099097,3.45490258866455));
#4846=CARTESIAN_POINT('',(-1.36599991081998,-0.000493598843714221,3.39184234729853));
#4847=CARTESIAN_POINT('Ctrl Pts',(-1.14737979714392,0.741266214733938,3.33530270583882));
#4848=CARTESIAN_POINT('Ctrl Pts',(-1.16553173502964,0.713169471087583,3.33749287913283));
#4849=CARTESIAN_POINT('Ctrl Pts',(-1.18265914426148,0.684394393768033,3.33970818833468));
#4850=CARTESIAN_POINT('Ctrl Pts',(-1.2088152291256,0.636525520319797,3.34337429489948));
#4851=CARTESIAN_POINT('Ctrl Pts',(-1.21847876351361,0.617825558236379,3.34480181944772));
#4852=CARTESIAN_POINT('Ctrl Pts',(-1.23337896702955,0.587281651913514,3.34713066806653));
#4853=CARTESIAN_POINT('Ctrl Pts',(-1.23888622487875,0.575573033670965,3.34802273391502));
#4854=CARTESIAN_POINT('Ctrl Pts',(-1.24920175812161,0.552807650407034,3.34975690199215));
#4855=CARTESIAN_POINT('Ctrl Pts',(-1.25403162017598,0.541761949615154,3.35059818068308));
#4856=CARTESIAN_POINT('Ctrl Pts',(-1.26506497396007,0.515590770887915,3.35259190912998));
#4857=CARTESIAN_POINT('Ctrl Pts',(-1.27114425800465,0.50041529309827,3.35374833556806));
#4858=CARTESIAN_POINT('Ctrl Pts',(-1.291535404168,0.446742671110167,3.35784152285206));
#4859=CARTESIAN_POINT('Ctrl Pts',(-1.30438099998516,0.407715971275957,3.36082422281042));
#4860=CARTESIAN_POINT('Ctrl Pts',(-1.34904172740674,0.248147434709551,3.37304616914902));
#4861=CARTESIAN_POINT('Ctrl Pts',(-1.36604493655855,0.124111950090538,3.38267270765495));
#4862=CARTESIAN_POINT('Ctrl Pts',(-1.36599991081998,-0.000493598843714221,
3.39184234729853));
#4863=CARTESIAN_POINT('Ctrl Pts',(-1.36599991021368,-0.000495273880241242,
3.39184247056333));
#4864=CARTESIAN_POINT('Ctrl Pts',(-1.36599590393764,-0.0115448626693739,
3.39265560201651));
#4865=CARTESIAN_POINT('Ctrl Pts',(-1.36585782719199,-0.0225944159718812,
3.39346426080702));
#4866=CARTESIAN_POINT('Ctrl Pts',(-1.36535745340085,-0.0429057471209498,
3.39494118066293));
#4867=CARTESIAN_POINT('Ctrl Pts',(-1.36503495032421,-0.0521677491801081,
3.3956110004149));
#4868=CARTESIAN_POINT('Ctrl Pts',(-1.36429798411226,-0.0685399176910465,
3.39678775934093));
#4869=CARTESIAN_POINT('Ctrl Pts',(-1.36392213285538,-0.0756513768739628,
3.39729647374242));
#4870=CARTESIAN_POINT('Ctrl Pts',(-1.36311177424707,-0.0890022657562773,
3.39824657357646));
#4871=CARTESIAN_POINT('Ctrl Pts',(-1.36268999543079,-0.0952422897295007,
3.39868860374223));
#4872=CARTESIAN_POINT('Ctrl Pts',(-1.36168841013103,-0.108687234500898,
3.3996363238915));
#4873=CARTESIAN_POINT('Ctrl Pts',(-1.36109424530452,-0.115890909044641,
3.40014121252018));
#4874=CARTESIAN_POINT('Ctrl Pts',(-1.35937157385279,-0.134930645165359,
3.40146881798367));
#4875=CARTESIAN_POINT('Ctrl Pts',(-1.35814564580875,-0.146757568167012,
3.40228648122653));
#4876=CARTESIAN_POINT('Ctrl Pts',(-1.35093711826357,-0.208436551116047,
3.40652114110718));
#4877=CARTESIAN_POINT('Ctrl Pts',(-1.34236309956909,-0.257952189750895,
3.40982029434804));
#4878=CARTESIAN_POINT('Ctrl Pts',(-1.30891028491174,-0.403048675850838,
3.41947895855282));
#4879=CARTESIAN_POINT('Ctrl Pts',(-1.27638634794584,-0.496519961800821,
3.4257101206697));
#4880=CARTESIAN_POINT('Ctrl Pts',(-1.22406380928573,-0.606769439937662,
3.43377357347458));
#4881=CARTESIAN_POINT('Ctrl Pts',(-1.2135123105183,-0.627605880511909,3.43533005965148));
#4882=CARTESIAN_POINT('Ctrl Pts',(-1.19310952938806,-0.665456002229991,
3.43822705981652));
#4883=CARTESIAN_POINT('Ctrl Pts',(-1.18341504237,-0.682547297101288,3.43956230899738));
#4884=CARTESIAN_POINT('Ctrl Pts',(-1.16687473620726,-0.71029540683938,3.44177888727376));
#4885=CARTESIAN_POINT('Ctrl Pts',(-1.16024314379836,-0.721077002636595,
3.44265260148688));
#4886=CARTESIAN_POINT('Ctrl Pts',(-1.1470036537035,-0.741946091713442,3.44436921744094));
#4887=CARTESIAN_POINT('Ctrl Pts',(-1.14041010181182,-0.75204133389026,3.44521154088886));
#4888=CARTESIAN_POINT('Ctrl Pts',(-1.12563396406584,-0.774023514954371,
3.44707278857188));
#4889=CARTESIAN_POINT('Ctrl Pts',(-1.11739499914696,-0.785870606613262,
3.44809372593308));
#4890=CARTESIAN_POINT('Ctrl Pts',(-1.08817729054475,-0.82649522359816,3.45165840230394));
#4891=CARTESIAN_POINT('Ctrl Pts',(-1.06626363181038,-0.854579215413105,
3.45423648440195));
#4892=CARTESIAN_POINT('Ctrl Pts',(-0.958663113371388,-0.981887973037428,
3.46647542244677));
#4893=CARTESIAN_POINT('Ctrl Pts',(-0.860093335543366,-1.06928526187117,
3.47661358361265));
#4894=CARTESIAN_POINT('Ctrl Pts',(-0.733445674074164,-1.15257745967072,
3.4877669224401));
#4895=CARTESIAN_POINT('Ctrl Pts',(-0.716042083561599,-1.16346946749612,
3.48926173826627));
#4896=CARTESIAN_POINT('Ctrl Pts',(-0.690769491677209,-1.1785042679643,3.49137217147332));
#4897=CARTESIAN_POINT('Ctrl Pts',(-0.683096150379825,-1.18296849513451,
3.49200518411794));
#4898=CARTESIAN_POINT('Ctrl Pts',(-0.670096600703223,-1.19036275376725,
3.49306389611154));
#4899=CARTESIAN_POINT('Ctrl Pts',(-0.664793574219285,-1.19333249718736,
3.49349197360485));
#4900=CARTESIAN_POINT('Ctrl Pts',(-0.652504229050625,-1.20010729082176,
3.49447514654437));
#4901=CARTESIAN_POINT('Ctrl Pts',(-0.645504247622066,-1.20388685211977,
3.49502868797276));
#4902=CARTESIAN_POINT('Ctrl Pts',(-0.625257865745741,-1.21459129155047,
3.49661234869313));
#4903=CARTESIAN_POINT('Ctrl Pts',(-0.61192985471768,-1.22136043104996,3.49763365570756));
#4904=CARTESIAN_POINT('Ctrl Pts',(-0.543687372610899,-1.25462234635429,
3.50276984381055));
#4905=CARTESIAN_POINT('Ctrl Pts',(-0.487148698063449,-1.27763883255426,
3.50672435641322));
#4906=CARTESIAN_POINT('Ctrl Pts',(-0.377227444142663,-1.31402396401995,
3.51418421326014));
#4907=CARTESIAN_POINT('Ctrl Pts',(-0.324210935829117,-1.32809889352064,
3.51768782599946));
#4908=CARTESIAN_POINT('Ctrl Pts',(-0.234467292565063,-1.34622876762799,
3.5236325436535));
#4909=CARTESIAN_POINT('Ctrl Pts',(-0.198164846547003,-1.3520492661629,3.52604046544842));
#4910=CARTESIAN_POINT('Ctrl Pts',(-0.134416205208806,-1.35964767799476,
3.53031418761997));
#4911=CARTESIAN_POINT('Ctrl Pts',(-0.107068639935826,-1.36207403084053,
3.53216184110225));
#4912=CARTESIAN_POINT('Ctrl Pts',(-0.0654976611379493,-1.36450267109421,
3.53500254817122));
#4913=CARTESIAN_POINT('Ctrl Pts',(-0.0513157789751146,-1.36510957370476,
3.53597726131334));
#4914=CARTESIAN_POINT('Ctrl Pts',(-0.0252719685231917,-1.36581769795545,
3.53777884746831));
#4915=CARTESIAN_POINT('Ctrl Pts',(-0.0134131268667021,-1.3659856254572,
3.53860359623135));
#4916=CARTESIAN_POINT('Ctrl Pts',(0.0127452574109342,-1.36601538249126,
3.54043329222531));
#4917=CARTESIAN_POINT('Ctrl Pts',(0.0270433075364403,-1.36580712355398,
3.54144029060256));
#4918=CARTESIAN_POINT('Ctrl Pts',(0.0684568887477681,-1.36455337976784,
3.54437820817033));
#4919=CARTESIAN_POINT('Ctrl Pts',(0.0955464838194545,-1.36292441382573,
3.54632646322206));
#4920=CARTESIAN_POINT('Ctrl Pts',(0.223030629400899,-1.35143923130649,3.55562546791917));
#4921=CARTESIAN_POINT('Ctrl Pts',(0.322169169590384,-1.33128952242584,3.56327227169015));
#4922=CARTESIAN_POINT('Ctrl Pts',(0.455203198504137,-1.28851056039669,3.57382485878223));
#4923=CARTESIAN_POINT('Ctrl Pts',(0.491714713228076,-1.27502407883675,3.57674892830087));
#4924=CARTESIAN_POINT('Ctrl Pts',(0.549601951149589,-1.25078476467622,3.58138684311496));
#4925=CARTESIAN_POINT('Ctrl Pts',(0.571357955372071,-1.24099761615838,3.58313023950591));
#4926=CARTESIAN_POINT('Ctrl Pts',(0.601302874754913,-1.22657202304881,3.58552000240874));
#4927=CARTESIAN_POINT('Ctrl Pts',(0.609715879559031,-1.22241181025489,3.58619028972989));
#4928=CARTESIAN_POINT('Ctrl Pts',(0.624118089656554,-1.21510426268439,3.58733500580171));
#4929=CARTESIAN_POINT('Ctrl Pts',(0.630127847530296,-1.21199862320992,3.58781181027507));
#4930=CARTESIAN_POINT('Ctrl Pts',(0.643123128445849,-1.20516030513938,3.58884077540917));
#4931=CARTESIAN_POINT('Ctrl Pts',(0.650099596850043,-1.20141135399056,3.58939195358872));
#4932=CARTESIAN_POINT('Ctrl Pts',(0.670000402713599,-1.19049312508178,3.5909618661344));
#4933=CARTESIAN_POINT('Ctrl Pts',(0.682841959688594,-1.18317425709462,3.59197202074394));
#4934=CARTESIAN_POINT('Ctrl Pts',(0.755582149701171,-1.14013810094253,3.59769223977836));
#4935=CARTESIAN_POINT('Ctrl Pts',(0.812801468170653,-1.10007970158708,3.60218837885737));
#4936=CARTESIAN_POINT('Ctrl Pts',(0.917105573820877,-1.01445722826584,3.61086776528305));
#4937=CARTESIAN_POINT('Ctrl Pts',(0.964466749904116,-0.969540828489386,
3.61504184624491));
#4938=CARTESIAN_POINT('Ctrl Pts',(1.03522581527352,-0.892098958042945,3.62193059556457));
#4939=CARTESIAN_POINT('Ctrl Pts',(1.06071960904808,-0.86163014194861,3.62457355439362));
#4940=CARTESIAN_POINT('Ctrl Pts',(1.09467192920382,-0.817258029479973,3.6283649546594));
#4941=CARTESIAN_POINT('Ctrl Pts',(1.10426633390737,-0.804246943399908,3.62947003048228));
#4942=CARTESIAN_POINT('Ctrl Pts',(1.12059310783276,-0.781262933244479,3.63141266985506));
#4943=CARTESIAN_POINT('Ctrl Pts',(1.12742893162224,-0.771365459600188,3.63224624312655));
#4944=CARTESIAN_POINT('Ctrl Pts',(1.14138492625693,-0.750576932412514,3.63399170797769));
#4945=CARTESIAN_POINT('Ctrl Pts',(1.1484819429641,-0.739671878146143,3.63490434229904));
#4946=CARTESIAN_POINT('Ctrl Pts',(1.16683910735932,-0.71056357912917,3.63733350796976));
#4947=CARTESIAN_POINT('Ctrl Pts',(1.17782864122889,-0.692194844544361,3.6388594965795));
#4948=CARTESIAN_POINT('Ctrl Pts',(1.23795244952326,-0.586119236691234,3.64763783672259));
#4949=CARTESIAN_POINT('Ctrl Pts',(1.27770942655118,-0.49347122671628,3.65520850989065));
#4950=CARTESIAN_POINT('Ctrl Pts',(1.32037549052948,-0.353126416749277,3.66630314156843));
#4951=CARTESIAN_POINT('Ctrl Pts',(1.33156146138188,-0.308276192986346,3.66979062979937));
#4952=CARTESIAN_POINT('Ctrl Pts',(1.34556562266081,-0.236884662234721,3.67518397886225));
#4953=CARTESIAN_POINT('Ctrl Pts',(1.34991674418092,-0.210680302780619,3.67713053355291));
#4954=CARTESIAN_POINT('Ctrl Pts',(1.35481762374498,-0.174700646966227,3.67974444137898));
#4955=CARTESIAN_POINT('Ctrl Pts',(1.35603039832201,-0.165023279093229,3.68044171414854));
#4956=CARTESIAN_POINT('Ctrl Pts',(1.3579143844052,-0.148562995015698,3.68161698966298));
#4957=CARTESIAN_POINT('Ctrl Pts',(1.35863865136182,-0.141786679083786,3.68209772654906));
#4958=CARTESIAN_POINT('Ctrl Pts',(1.36007574950981,-0.127317083786312,3.68311739354062));
#4959=CARTESIAN_POINT('Ctrl Pts',(1.36077407516135,-0.11962277366247,3.68365555954664));
#4960=CARTESIAN_POINT('Ctrl Pts',(1.3625435325228,-0.0980994234155056,3.68515070585198));
#4961=CARTESIAN_POINT('Ctrl Pts',(1.36346941298701,-0.0842589563290845,
3.68610032068763));
#4962=CARTESIAN_POINT('Ctrl Pts',(1.36853611040705,0.0139130226736218,3.69276751680514));
#4963=CARTESIAN_POINT('Ctrl Pts',(1.36506151870747,0.0984655037191526,3.6981594842981));
#4964=CARTESIAN_POINT('Ctrl Pts',(1.34626919687876,0.23812495429526,3.70721932970824));
#4965=CARTESIAN_POINT('Ctrl Pts',(1.33527715486039,0.293561904997251,3.71085588256634));
#4966=CARTESIAN_POINT('Ctrl Pts',(1.31158314690899,0.383455632897793,3.71697984121087));
#4967=CARTESIAN_POINT('Ctrl Pts',(1.30086864009321,0.418364668187871,3.71941589234884));
#4968=CARTESIAN_POINT('Ctrl Pts',(1.28356289872946,0.467620604524368,3.72296258118187));
#4969=CARTESIAN_POINT('Ctrl Pts',(1.27810093328913,0.482349162796248,3.72403739850416));
#4970=CARTESIAN_POINT('Ctrl Pts',(1.268032640941,0.50812638564804,3.72594563063877));
#4971=CARTESIAN_POINT('Ctrl Pts',(1.26353273571693,0.519214996137751,3.72677549200968));
#4972=CARTESIAN_POINT('Ctrl Pts',(1.25375755346116,0.542422966530153,3.72853214012195));
#4973=CARTESIAN_POINT('Ctrl Pts',(1.2484509209254,0.554527685322951,3.72945989966749));
#4974=CARTESIAN_POINT('Ctrl Pts',(1.23366978006981,0.586956257984964,3.73197764540899));
#4975=CARTESIAN_POINT('Ctrl Pts',(1.22386947130074,0.6071261707956,3.73357837087617));
#4976=CARTESIAN_POINT('Ctrl Pts',(1.17449220752656,0.702690557446264,3.74133560899769));
#4977=CARTESIAN_POINT('Ctrl Pts',(1.12842558306736,0.774504603228048,3.74770851068264));
#4978=CARTESIAN_POINT('Ctrl Pts',(1.04165183636111,0.885450800707789,3.75835788231333));
#4979=CARTESIAN_POINT('Ctrl Pts',(1.00466374234151,0.927207042255812,3.76258409997924));
#4980=CARTESIAN_POINT('Ctrl Pts',(0.94426543338702,0.987520293450898,3.76893167161489));
#4981=CARTESIAN_POINT('Ctrl Pts',(0.92262669958857,1.00776673976217,3.77110945391525));
#4982=CARTESIAN_POINT('Ctrl Pts',(0.892730303081213,1.03396862930749,3.77397442990409));
#4983=CARTESIAN_POINT('Ctrl Pts',(0.88504139699246,1.04055766863373,3.77469908113244));
#4984=CARTESIAN_POINT('Ctrl Pts',(0.872009912232269,1.0514760945688,3.77590599794318));
#4985=CARTESIAN_POINT('Ctrl Pts',(0.866706726745205,1.05585165765819,3.77639136204842));
#4986=CARTESIAN_POINT('Ctrl Pts',(0.855500007999725,1.06495678169794,3.77740462625131));
#4987=CARTESIAN_POINT('Ctrl Pts',(0.849589884403435,1.06967763642221,3.77793195413955));
#4988=CARTESIAN_POINT('Ctrl Pts',(0.833041458879929,1.08267240904025,3.77938999568114));
#4989=CARTESIAN_POINT('Ctrl Pts',(0.822319152640842,1.09083860538404,3.78031375946463));
#4990=CARTESIAN_POINT('Ctrl Pts',(0.739502471477243,1.15199722447806,3.78730551441112));
#4991=CARTESIAN_POINT('Ctrl Pts',(0.662469481435449,1.19795662710755,3.79300179560354));
#4992=CARTESIAN_POINT('Ctrl Pts',(0.508495851634213,1.27039145424832,3.80394614091116));
#4993=CARTESIAN_POINT('Ctrl Pts',(0.432617423839096,1.29819198807891,3.80916299178731));
#4994=CARTESIAN_POINT('Ctrl Pts',(0.336132386309956,1.3241382520869,3.81589928524886));
#4995=CARTESIAN_POINT('Ctrl Pts',(0.317426613634589,1.32874654299215,3.81720918059708));
#4996=CARTESIAN_POINT('Ctrl Pts',(0.286353251965,1.33570809263181,3.81939503016453));
#4997=CARTESIAN_POINT('Ctrl Pts',(0.274039060475738,1.33828878377039,3.8202638004783));
#4998=CARTESIAN_POINT('Ctrl Pts',(0.249809535384183,1.34301815016927,3.82197904448198));
#4999=CARTESIAN_POINT('Ctrl Pts',(0.237897790069512,1.34517923731474,3.82282504374344));
#5000=CARTESIAN_POINT('Ctrl Pts',(0.20880856103766,1.35005829695095,3.8248984743046));
#5001=CARTESIAN_POINT('Ctrl Pts',(0.191605266156183,1.3526070356324,3.82613100596007));
#5002=CARTESIAN_POINT('Ctrl Pts',(0.128238249493952,1.36076202019167,3.83069628795973));
#5003=CARTESIAN_POINT('Ctrl Pts',(0.0818499355370338,1.36433795355393,3.83408895335321));
#5004=CARTESIAN_POINT('Ctrl Pts',(-0.0811414757157418,1.368560200967,3.84617946892474));
#5005=CARTESIAN_POINT('Ctrl Pts',(-0.19755208203603,1.35665440610863,3.85516547647375));
#5006=CARTESIAN_POINT('Ctrl Pts',(-0.331179380679531,1.32540722161005,3.86526526453535));
#5007=CARTESIAN_POINT('Ctrl Pts',(-0.351217838482758,1.32023870093808,3.86677226365154));
#5008=CARTESIAN_POINT('Ctrl Pts',(-0.37970093514585,1.31219757332659,3.86889652713996));
#5009=CARTESIAN_POINT('Ctrl Pts',(-0.388245927499615,1.30969476687042,3.86953148534938));
#5010=CARTESIAN_POINT('Ctrl Pts',(-0.402584791431123,1.30534227775591,3.87059236111436));
#5011=CARTESIAN_POINT('Ctrl Pts',(-0.408391666412527,1.30353719877729,3.87102068167333));
#5012=CARTESIAN_POINT('Ctrl Pts',(-0.421749818543827,1.2992867595422,3.87200287326152));
#5013=CARTESIAN_POINT('Ctrl Pts',(-0.429292111715352,1.2968142826657,3.87255520914989));
#5014=CARTESIAN_POINT('Ctrl Pts',(-0.450893441651801,1.28952392612613,3.87413184967456));
#5015=CARTESIAN_POINT('Ctrl Pts',(-0.464896449607035,1.28454201474701,3.8751474611269));
#5016=CARTESIAN_POINT('Ctrl Pts',(-0.539905106977256,1.25646850381103,3.8805670161767));
#5017=CARTESIAN_POINT('Ctrl Pts',(-0.599285387177935,1.22925571090017,3.88478546734755));
#5018=CARTESIAN_POINT('Ctrl Pts',(-0.71631776752998,1.16511710113681,3.89337526959117));
#5019=CARTESIAN_POINT('Ctrl Pts',(-0.773594151092775,1.12790095317371,3.8977345822808));
#5020=CARTESIAN_POINT('Ctrl Pts',(-0.860239278385417,1.06188625681575,3.90488121619118));
#5021=CARTESIAN_POINT('Ctrl Pts',(-0.891506318635939,1.03577509280707,3.90758897541789));
#5022=CARTESIAN_POINT('Ctrl Pts',(-0.933591065331616,0.997311106591054,
3.91145666486047));
#5023=CARTESIAN_POINT('Ctrl Pts',(-0.945425281133438,0.98609975171272,3.91257071098413));
#5024=CARTESIAN_POINT('Ctrl Pts',(-0.965652492257582,0.966238287242019,
3.91452367020683));
#5025=CARTESIAN_POINT('Ctrl Pts',(-0.974137048655124,0.957683746254458,
3.91535846228015));
#5026=CARTESIAN_POINT('Ctrl Pts',(-0.99150868888105,0.939699098821539,3.91710122539235));
#5027=CARTESIAN_POINT('Ctrl Pts',(-1.00037693777964,0.930252566967899,3.91800987610551));
#5028=CARTESIAN_POINT('Ctrl Pts',(-1.0233546244042,0.905067969813148,3.92041577486997));
#5029=CARTESIAN_POINT('Ctrl Pts',(-1.0372349984114,0.889126642916958,3.92192215404341));
#5030=CARTESIAN_POINT('Ctrl Pts',(-1.0855819584618,0.830927800972093,3.92736687910065));
#5031=CARTESIAN_POINT('Ctrl Pts',(-1.11784827311584,0.786977040024542,3.93138133830545));
#5032=CARTESIAN_POINT('Ctrl Pts',(-1.14737996054503,0.741265961811063,3.93545337707765));
#5033=CARTESIAN_POINT('Origin',(0.,0.,-1.10921167016993));
#5034=CARTESIAN_POINT('',(-1.14737959883991,0.741266521681617,4.6555522104354));
#5035=CARTESIAN_POINT('',(-1.1473796037955,0.741266514011044,4.53716884124631));
#5036=CARTESIAN_POINT('',(-1.14737960344596,0.741266514552077,-1.10921167016993));
#5037=CARTESIAN_POINT('',(-1.36599977587709,-0.000782498403878971,4.11011263784981));
#5038=CARTESIAN_POINT('Ctrl Pts',(-1.14737959883991,0.741266521681617,4.6555522104354));
#5039=CARTESIAN_POINT('Ctrl Pts',(-1.13681643246464,0.757616864296101,4.65414490266099));
#5040=CARTESIAN_POINT('Ctrl Pts',(-1.1259043798636,0.773740481038852,4.6527258208392));
#5041=CARTESIAN_POINT('Ctrl Pts',(-1.08172649896303,0.83610277291328,4.6471130366888));
#5042=CARTESIAN_POINT('Ctrl Pts',(-1.04593062863914,0.880470380959298,4.64284200642283));
#5043=CARTESIAN_POINT('Ctrl Pts',(-0.951056440806476,0.98408693736181,4.63222931054489));
#5044=CARTESIAN_POINT('Ctrl Pts',(-0.889101729298465,1.04040165390782,4.6258675472562));
#5045=CARTESIAN_POINT('Ctrl Pts',(-0.811250672179,1.09910091524944,4.61877142843508));
#5046=CARTESIAN_POINT('Ctrl Pts',(-0.799987245637843,1.10732602239255,4.61776500923298));
#5047=CARTESIAN_POINT('Ctrl Pts',(-0.78227681786195,1.11984772900455,4.61621603862062));
#5048=CARTESIAN_POINT('Ctrl Pts',(-0.775916248168164,1.12426417679661,4.6156663068812));
#5049=CARTESIAN_POINT('Ctrl Pts',(-0.763889898073782,1.13246396359275,4.61463967784272));
#5050=CARTESIAN_POINT('Ctrl Pts',(-0.758233111151425,1.13625919425788,4.61416208127374));
#5051=CARTESIAN_POINT('Ctrl Pts',(-0.744432702333554,1.14536915625704,4.61300926228246));
#5052=CARTESIAN_POINT('Ctrl Pts',(-0.736260312412042,1.15063952594443,4.61233684099016));
#5053=CARTESIAN_POINT('Ctrl Pts',(-0.705759840928751,1.16985123280071,4.60986229597919));
#5054=CARTESIAN_POINT('Ctrl Pts',(-0.683085057620925,1.18323449780022,4.60809138498994));
#5055=CARTESIAN_POINT('Ctrl Pts',(-0.620180296323417,1.21795102444348,4.60332312854167));
#5056=CARTESIAN_POINT('Ctrl Pts',(-0.579247259535045,1.23794242849322,4.60037567311025));
#5057=CARTESIAN_POINT('Ctrl Pts',(-0.443810095535263,1.29589709102148,4.59088609784645));
#5058=CARTESIAN_POINT('Ctrl Pts',(-0.346057739725599,1.32535220373791,4.58440798163169));
#5059=CARTESIAN_POINT('Ctrl Pts',(-0.225042257599612,1.3475027011048,4.57614248565504));
#5060=CARTESIAN_POINT('Ctrl Pts',(-0.204054451250564,1.35084020051338,4.574701642616));
#5061=CARTESIAN_POINT('Ctrl Pts',(-0.170133159265685,1.35542585307797,4.57235639167771));
#5062=CARTESIAN_POINT('Ctrl Pts',(-0.157244331800852,1.3569814793507,4.57146148718378));
#5063=CARTESIAN_POINT('Ctrl Pts',(-0.132359519535727,1.35962568561049,4.56972537298692));
#5064=CARTESIAN_POINT('Ctrl Pts',(-0.120367421591689,1.3607397675028,4.56888503404971));
#5065=CARTESIAN_POINT('Ctrl Pts',(-0.0921632903585972,1.36298422728454,
4.56689921662262));
#5066=CARTESIAN_POINT('Ctrl Pts',(-0.0759430267644908,1.36398412460856,
4.56574985641495));
#5067=CARTESIAN_POINT('Ctrl Pts',(-0.0194266633236217,1.36645688151918,
4.56171784915685));
#5068=CARTESIAN_POINT('Ctrl Pts',(0.0209103912782695,1.36643477079933,4.55879111787919));
#5069=CARTESIAN_POINT('Ctrl Pts',(0.128114878321844,1.36162818728456,4.55088143233744));
#5070=CARTESIAN_POINT('Ctrl Pts',(0.194728674362897,1.35370749435882,4.54582596883842));
#5071=CARTESIAN_POINT('Ctrl Pts',(0.325920811446947,1.32822244903224,4.53571621447658));
#5072=CARTESIAN_POINT('Ctrl Pts',(0.390342837070776,1.31073766780952,4.53067607025463));
#5073=CARTESIAN_POINT('Ctrl Pts',(0.467436171292611,1.28362223534042,4.52471499749282));
#5074=CARTESIAN_POINT('Ctrl Pts',(0.481554408691499,1.27839274705169,4.52362657289817));
#5075=CARTESIAN_POINT('Ctrl Pts',(0.503018878159732,1.27003608765898,4.52197971303324));
#5076=CARTESIAN_POINT('Ctrl Pts',(0.510428475592943,1.26707633359795,4.52141267539273));
#5077=CARTESIAN_POINT('Ctrl Pts',(0.52343477606493,1.26174837304377,4.52042044274694));
#5078=CARTESIAN_POINT('Ctrl Pts',(0.529042004989777,1.25940759127332,4.51999374761097));
#5079=CARTESIAN_POINT('Ctrl Pts',(0.542776754327717,1.25356599260113,4.51895100167646));
#5080=CARTESIAN_POINT('Ctrl Pts',(0.550886169778131,1.25002349637814,4.51833738146309));
#5081=CARTESIAN_POINT('Ctrl Pts',(0.5775261024892,1.23807656762518,4.51632654325638));
#5082=CARTESIAN_POINT('Ctrl Pts',(0.595904209868544,1.2293365142362,4.51494726991068));
#5083=CARTESIAN_POINT('Ctrl Pts',(0.7304104455655,1.16164388859076,4.50486205028363));
#5084=CARTESIAN_POINT('Ctrl Pts',(0.837779074871426,1.08676111512157,4.49680444163767));
#5085=CARTESIAN_POINT('Ctrl Pts',(0.959489801573599,0.972963350166433,4.48583621152266));
#5086=CARTESIAN_POINT('Ctrl Pts',(0.985047900184815,0.947079005440055,4.48341176641356));
#5087=CARTESIAN_POINT('Ctrl Pts',(1.01933962101197,0.909458239407976,4.47995731823536));
#5088=CARTESIAN_POINT('Ctrl Pts',(1.02896512996194,0.898553441101538,4.47896371240582));
#5089=CARTESIAN_POINT('Ctrl Pts',(1.04626719573852,0.878309196263678,4.47713149029872));
#5090=CARTESIAN_POINT('Ctrl Pts',(1.05399748853746,0.869017472231356,4.47629513664676));
#5091=CARTESIAN_POINT('Ctrl Pts',(1.06954465518556,0.849817321543008,4.47457542698254));
#5092=CARTESIAN_POINT('Ctrl Pts',(1.07734952679881,0.839900724881466,4.47369170978825));
#5093=CARTESIAN_POINT('Ctrl Pts',(1.0968280738694,0.814433684968138,4.47143263039334));
#5094=CARTESIAN_POINT('Ctrl Pts',(1.10830882513432,0.798739963982603,4.47005010274079));
#5095=CARTESIAN_POINT('Ctrl Pts',(1.13264863027497,0.763932928039307,4.4670028050395));
#5096=CARTESIAN_POINT('Ctrl Pts',(1.14536687068168,0.744728851046618,4.46533351654632));
#5097=CARTESIAN_POINT('Ctrl Pts',(1.18328761437629,0.684199376747995,4.46010817097348));
#5098=CARTESIAN_POINT('Ctrl Pts',(1.20678213764331,0.641852379674511,4.4565016010922));
#5099=CARTESIAN_POINT('Ctrl Pts',(1.26999417017976,0.512124274974056,4.44564099771009));
#5100=CARTESIAN_POINT('Ctrl Pts',(1.30281216369449,0.421709056477101,4.43829572754769));
#5101=CARTESIAN_POINT('Ctrl Pts',(1.32942669054545,0.314320016964369,4.43023094353458));
#5102=CARTESIAN_POINT('Ctrl Pts',(1.33273468117738,0.29998452002598,4.42916793594976));
#5103=CARTESIAN_POINT('Ctrl Pts',(1.33746363795136,0.277866025369277,4.42755133915668));
#5104=CARTESIAN_POINT('Ctrl Pts',(1.33904956777796,0.270119924939434,4.42698959938482));
#5105=CARTESIAN_POINT('Ctrl Pts',(1.341868480566,0.255716276301144,4.42595376099447));
#5106=CARTESIAN_POINT('Ctrl Pts',(1.34311930527297,0.249062978836249,4.42547878321777));
#5107=CARTESIAN_POINT('Ctrl Pts',(1.34599134840036,0.233134994403005,4.42434966150155));
#5108=CARTESIAN_POINT('Ctrl Pts',(1.34756623140728,0.223852407307993,4.42369801386201));
#5109=CARTESIAN_POINT('Ctrl Pts',(1.35282233699995,0.1908037341714,4.42139823026359));
#5110=CARTESIAN_POINT('Ctrl Pts',(1.35597202933726,0.166956171167324,4.41977585413383));
#5111=CARTESIAN_POINT('Ctrl Pts',(1.36261666114558,0.103848588476881,4.41555083998215));
#5112=CARTESIAN_POINT('Ctrl Pts',(1.36504545563517,0.0644981095171581,4.41298530146863));
#5113=CARTESIAN_POINT('Ctrl Pts',(1.36765996790229,-0.0777920679294303,
4.4037896401327));
#5114=CARTESIAN_POINT('Ctrl Pts',(1.35791888273026,-0.180555856577663,4.39727444877455));
#5115=CARTESIAN_POINT('Ctrl Pts',(1.33195221857356,-0.30397104968724,4.38885948732663));
#5116=CARTESIAN_POINT('Ctrl Pts',(1.3265933442415,-0.326565628578373,4.38729538207649));
#5117=CARTESIAN_POINT('Ctrl Pts',(1.3169170553905,-0.363180744624295,4.38471535134865));
#5118=CARTESIAN_POINT('Ctrl Pts',(1.31294493195247,-0.37728816786237,4.38371016219692));
#5119=CARTESIAN_POINT('Ctrl Pts',(1.3053452573232,-0.40270428043604,4.3818775052349));
#5120=CARTESIAN_POINT('Ctrl Pts',(1.3017957078565,-0.414034899214241,4.38105259665002));
#5121=CARTESIAN_POINT('Ctrl Pts',(1.29377502551484,-0.438514587195286,4.37925244511929));
#5122=CARTESIAN_POINT('Ctrl Pts',(1.28925019547755,-0.451644515137716,4.37827554829125));
#5123=CARTESIAN_POINT('Ctrl Pts',(1.27574494493506,-0.488975576304179,4.37546423455226));
#5124=CARTESIAN_POINT('Ctrl Pts',(1.26627810241333,-0.512993067533084,4.37361435210378));
#5125=CARTESIAN_POINT('Ctrl Pts',(1.23606819680581,-0.583695328186959,4.3680413947036));
#5126=CARTESIAN_POINT('Ctrl Pts',(1.21338284804615,-0.62949653486628,4.36426009006419));
#5127=CARTESIAN_POINT('Ctrl Pts',(1.14783121367799,-0.745071361790101,4.35429497627933));
#5128=CARTESIAN_POINT('Ctrl Pts',(1.10116444459002,-0.812455839623985,4.34804675116188));
#5129=CARTESIAN_POINT('Ctrl Pts',(1.02902102992214,-0.898899197982087,4.33966077509498));
#5130=CARTESIAN_POINT('Ctrl Pts',(1.00849684888504,-0.92186683995035,4.3373933838686));
#5131=CARTESIAN_POINT('Ctrl Pts',(0.979925962112418,-0.951741690410964,
4.33441056898041));
#5132=CARTESIAN_POINT('Ctrl Pts',(0.972551431938664,-0.959276220021634,
4.33365529095072));
#5133=CARTESIAN_POINT('Ctrl Pts',(0.960218942040365,-0.97158785501711,4.33241723406193));
#5134=CARTESIAN_POINT('Ctrl Pts',(0.955310882376777,-0.976414104141062,
4.3319308922147));
#5135=CARTESIAN_POINT('Ctrl Pts',(0.945055027142969,-0.986347641615543,
4.33092813061226));
#5136=CARTESIAN_POINT('Ctrl Pts',(0.939701889510002,-0.991448959784946,
4.33041213613678));
#5137=CARTESIAN_POINT('Ctrl Pts',(0.925068266991029,-1.0051691908097,4.32902063739346));
#5138=CARTESIAN_POINT('Ctrl Pts',(0.915708659453455,-1.01370315212288,4.32815108288754));
#5139=CARTESIAN_POINT('Ctrl Pts',(0.894272035590667,-1.03270953492134,4.3262014641812));
#5140=CARTESIAN_POINT('Ctrl Pts',(0.882127040891523,-1.04310276954036,4.32512606377035));
#5141=CARTESIAN_POINT('Ctrl Pts',(0.841344647310729,-1.07678096719485,4.32159919205269));
#5142=CARTESIAN_POINT('Ctrl Pts',(0.811944801192098,-1.09911967552151,4.3191902522613));
#5143=CARTESIAN_POINT('Ctrl Pts',(0.688244605706175,-1.185434359558,4.30942702802883));
#5144=CARTESIAN_POINT('Ctrl Pts',(0.5870344929767,-1.23867846599605,4.30223992629826));
#5145=CARTESIAN_POINT('Ctrl Pts',(0.460069897703798,-1.28637588929564,4.29313469518001));
#5146=CARTESIAN_POINT('Ctrl Pts',(0.439570429978327,-1.29352425204126,4.29166366973095));
#5147=CARTESIAN_POINT('Ctrl Pts',(0.406465475513297,-1.30419046404805,4.28928159701591));
#5148=CARTESIAN_POINT('Ctrl Pts',(0.393964168330396,-1.30802108663231,4.28838062272838));
#5149=CARTESIAN_POINT('Ctrl Pts',(0.369876287948202,-1.31502540285413,4.28664083163194));
#5150=CARTESIAN_POINT('Ctrl Pts',(0.358299013010455,-1.31822686955318,4.28580299253496));
#5151=CARTESIAN_POINT('Ctrl Pts',(0.331178906505499,-1.32534274913988,4.2838357449521));
#5152=CARTESIAN_POINT('Ctrl Pts',(0.315606697845275,-1.32913702991996,4.28270266753585));
#5153=CARTESIAN_POINT('Ctrl Pts',(0.262221462452358,-1.34115368472101,4.27880454595813));
#5154=CARTESIAN_POINT('Ctrl Pts',(0.224130576277147,-1.34804238554939,4.27599931312125));
#5155=CARTESIAN_POINT('Ctrl Pts',(0.124094649932641,-1.36177680421504,4.26856851591045));
#5156=CARTESIAN_POINT('Ctrl Pts',(0.0618856865027673,-1.36601771434405,
4.26388176148126));
#5157=CARTESIAN_POINT('Ctrl Pts',(-0.0748175337652816,-1.3659787068457,
4.25354350693301));
#5158=CARTESIAN_POINT('Ctrl Pts',(-0.149125041604392,-1.35987463167423,
4.24789735128025));
#5159=CARTESIAN_POINT('Ctrl Pts',(-0.236919152496719,-1.34537609042737,
4.24141320960069));
#5160=CARTESIAN_POINT('Ctrl Pts',(-0.251230151135062,-1.34277733201691,
4.24036256969299));
#5161=CARTESIAN_POINT('Ctrl Pts',(-0.273218541546837,-1.33842055483616,
4.23876072398793));
#5162=CARTESIAN_POINT('Ctrl Pts',(-0.28092634628775,-1.33682397825462,4.23820158388203));
#5163=CARTESIAN_POINT('Ctrl Pts',(-0.295245046626378,-1.33372872146579,
4.23716782325992));
#5164=CARTESIAN_POINT('Ctrl Pts',(-0.301858932691299,-1.33224739714465,
4.23669236209439));
#5165=CARTESIAN_POINT('Ctrl Pts',(-0.317694402964717,-1.32857671387481,
4.23555848812507));
#5166=CARTESIAN_POINT('Ctrl Pts',(-0.326904673722462,-1.32634051644428,
4.2349026332455));
#5167=CARTESIAN_POINT('Ctrl Pts',(-0.359831502033754,-1.31798224798194,
4.2325685325624));
#5168=CARTESIAN_POINT('Ctrl Pts',(-0.38340713535126,-1.3113180620359,4.23091707357985));
#5169=CARTESIAN_POINT('Ctrl Pts',(-0.445503517139512,-1.29194697747711,
4.22658895415234));
#5170=CARTESIAN_POINT('Ctrl Pts',(-0.483660300729215,-1.27815238628299,
4.22395166915638));
#5171=CARTESIAN_POINT('Ctrl Pts',(-0.620688760291736,-1.22159627851947,
4.21437971757785));
#5172=CARTESIAN_POINT('Ctrl Pts',(-0.71501261877081,-1.16889141522903,4.20755944987793));
#5173=CARTESIAN_POINT('Ctrl Pts',(-0.820011769853555,-1.09271347013798,
4.19885552123938));
#5174=CARTESIAN_POINT('Ctrl Pts',(-0.837539286400239,-1.07933770648205,
4.19736224866106));
#5175=CARTESIAN_POINT('Ctrl Pts',(-0.864986868265193,-1.05732041342426,
4.19495302376748));
#5176=CARTESIAN_POINT('Ctrl Pts',(-0.875119499246772,-1.04894927444347,
4.19404757277319));
#5177=CARTESIAN_POINT('Ctrl Pts',(-0.894262513316769,-1.03266371052275,
4.19230486194445));
#5178=CARTESIAN_POINT('Ctrl Pts',(-0.903292589406051,-1.02477425005016,
4.19146865663819));
#5179=CARTESIAN_POINT('Ctrl Pts',(-0.924033494738829,-1.00616604222044,
4.18951402617379));
#5180=CARTESIAN_POINT('Ctrl Pts',(-0.935663444940012,-0.995360178040924,
4.18839207664489));
#5181=CARTESIAN_POINT('Ctrl Pts',(-0.974213788749859,-0.958268755222606,
4.18458256971323));
#5182=CARTESIAN_POINT('Ctrl Pts',(-1.00023379076665,-0.931076475877344,
4.18185729477677));
#5183=CARTESIAN_POINT('Ctrl Pts',(-1.06433567242301,-0.858294939275736,
4.17472770586481));
#5184=CARTESIAN_POINT('Ctrl Pts',(-1.10062520476704,-0.8112358428113,4.17026870815185));
#5185=CARTESIAN_POINT('Ctrl Pts',(-1.17802757691521,-0.696068789739845,
4.15978016187041));
#5186=CARTESIAN_POINT('Ctrl Pts',(-1.21649205425785,-0.626426182775873,
4.15374414733136));
#5187=CARTESIAN_POINT('Ctrl Pts',(-1.25444773757453,-0.540849841815934,
4.14692715153952));
#5188=CARTESIAN_POINT('Ctrl Pts',(-1.26000302676748,-0.527778448052726,
4.1459018126505));
#5189=CARTESIAN_POINT('Ctrl Pts',(-1.26829155491539,-0.50739860312754,4.14433019460683));
#5190=CARTESIAN_POINT('Ctrl Pts',(-1.27116757610949,-0.500149789361644,
4.14377641621747));
#5191=CARTESIAN_POINT('Ctrl Pts',(-1.27643366120105,-0.486538074328516,
4.1427467984679));
#5192=CARTESIAN_POINT('Ctrl Pts',(-1.27883844365662,-0.480181659896265,
4.14227019862244));
#5193=CARTESIAN_POINT('Ctrl Pts',(-1.28453041719027,-0.464790308060041,
4.14112588309805));
#5194=CARTESIAN_POINT('Ctrl Pts',(-1.28776983832396,-0.455738170571644,
4.14046085980594));
#5195=CARTESIAN_POINT('Ctrl Pts',(-1.29924798291507,-0.422564058269026,
4.13805012019792));
#5196=CARTESIAN_POINT('Ctrl Pts',(-1.30690721005451,-0.398245456948158,
4.13633356127149));
#5197=CARTESIAN_POINT('Ctrl Pts',(-1.34838760953678,-0.252415373972079,
4.12625992727964));
#5198=CARTESIAN_POINT('Ctrl Pts',(-1.3659275236544,-0.126912493698488,4.11843313937027));
#5199=CARTESIAN_POINT('Ctrl Pts',(-1.36599977587709,-0.000782498403878971,
4.11011263784981));
#5200=CARTESIAN_POINT('Ctrl Pts',(-1.36599977678399,-0.000780913632299608,
4.1101125333061));
#5201=CARTESIAN_POINT('Ctrl Pts',(-1.36601137218235,0.0195021380629541,
4.10877450718365));
#5202=CARTESIAN_POINT('Ctrl Pts',(-1.36557120786974,0.0397823578990402,
4.10742655868002));
#5203=CARTESIAN_POINT('Ctrl Pts',(-1.36397231189203,0.0761215963178287,
4.10498718936274));
#5204=CARTESIAN_POINT('Ctrl Pts',(-1.36298093129678,0.0921841185697551,
4.10390051557796));
#5205=CARTESIAN_POINT('Ctrl Pts',(-1.36075157624018,0.120234292919318,4.10198572787291));
#5206=CARTESIAN_POINT('Ctrl Pts',(-1.35963829236043,0.132230238279988,4.10116136067351));
#5207=CARTESIAN_POINT('Ctrl Pts',(-1.35718028794476,0.155383145088946,4.09955876113539));
#5208=CARTESIAN_POINT('Ctrl Pts',(-1.35585626841899,0.166541352542645,4.09878121928405));
#5209=CARTESIAN_POINT('Ctrl Pts',(-1.35276476363943,0.190106629894382,4.09712745553751));
#5210=CARTESIAN_POINT('Ctrl Pts',(-1.35096389741556,0.202508187176493,4.09625027262785));
#5211=CARTESIAN_POINT('Ctrl Pts',(-1.34600440558525,0.233642910845264,4.09402991284754));
#5212=CARTESIAN_POINT('Ctrl Pts',(-1.34262522273736,0.252337703479607,4.09268006163803));
#5213=CARTESIAN_POINT('Ctrl Pts',(-1.32449797592249,0.341908983755579,4.08612884092479));
#5214=CARTESIAN_POINT('Ctrl Pts',(-1.30452318297912,0.411598060741742,4.08076902519247));
#5215=CARTESIAN_POINT('Ctrl Pts',(-1.24858407822589,0.560863874792138,4.06877243336367));
#5216=CARTESIAN_POINT('Ctrl Pts',(-1.21032339876078,0.639256304739435,4.06212012760547));
#5217=CARTESIAN_POINT('Ctrl Pts',(-1.15914692479946,0.722809922827223,4.05490893509864));
#5218=CARTESIAN_POINT('Ctrl Pts',(-1.1533186175403,0.732073729638883,4.05410786115583));
#5219=CARTESIAN_POINT('Ctrl Pts',(-1.14737960320835,0.741266514919876,4.0533120739516));
#5220=CARTESIAN_POINT('Ctrl Pts',(-1.14737996054503,0.741265961811063,3.93545337707765));
#5221=CARTESIAN_POINT('Ctrl Pts',(-1.17686458301595,0.695627733819701,3.9395189261992));
#5222=CARTESIAN_POINT('Ctrl Pts',(-1.20362337238171,0.64823483442225,3.94364170049026));
#5223=CARTESIAN_POINT('Ctrl Pts',(-1.24542367906319,0.562622997095374,3.95084044159456));
#5224=CARTESIAN_POINT('Ctrl Pts',(-1.26169221740402,0.525126553894161,3.95391492532671));
#5225=CARTESIAN_POINT('Ctrl Pts',(-1.2823143737366,0.471078161299187,3.95819399034062));
#5226=CARTESIAN_POINT('Ctrl Pts',(-1.28807583568596,0.455088435384634,3.95944149461941));
#5227=CARTESIAN_POINT('Ctrl Pts',(-1.2978007737332,0.426433018885614,3.96163992568542));
#5228=CARTESIAN_POINT('Ctrl Pts',(-1.30188086972375,0.413809379061976,3.96259574175867));
#5229=CARTESIAN_POINT('Ctrl Pts',(-1.30798474047843,0.393939668809511,3.96407838463171));
#5230=CARTESIAN_POINT('Ctrl Pts',(-1.31013355021347,0.386733282114039,3.96461165791519));
#5231=CARTESIAN_POINT('Ctrl Pts',(-1.3141163828407,0.372961910005135,3.96562179630003));
#5232=CARTESIAN_POINT('Ctrl Pts',(-1.31596093938591,0.366400412343076,3.96609919001826));
#5233=CARTESIAN_POINT('Ctrl Pts',(-1.32000247667041,0.351599446310775,3.96716781213017));
#5234=CARTESIAN_POINT('Ctrl Pts',(-1.32217160980735,0.343352519509725,3.96775752826322));
#5235=CARTESIAN_POINT('Ctrl Pts',(-1.32977416240038,0.313307110930736,3.96988712136449));
#5236=CARTESIAN_POINT('Ctrl Pts',(-1.3347471792539,0.29139453280524,3.97140432418455));
#5237=CARTESIAN_POINT('Ctrl Pts',(-1.3569392860437,0.181065183732163,3.97890981395983));
#5238=CARTESIAN_POINT('Ctrl Pts',(-1.36592523621316,0.091214549048413,3.98460781304651));
#5239=CARTESIAN_POINT('Ctrl Pts',(-1.3660542545431,-0.065220445816803,3.99470471777367));
#5240=CARTESIAN_POINT('Ctrl Pts',(-1.3612753222363,-0.131475850328248,3.99903426838739));
#5241=CARTESIAN_POINT('Ctrl Pts',(-1.34897092127529,-0.215851565304085,
4.00478679124949));
#5242=CARTESIAN_POINT('Ctrl Pts',(-1.34584982351778,-0.234526414197535,
4.00607482564002));
#5243=CARTESIAN_POINT('Ctrl Pts',(-1.34002235318472,-0.265429381020699,
4.00823424120534));
#5244=CARTESIAN_POINT('Ctrl Pts',(-1.33753407816726,-0.277696300204813,
4.00909880321475));
#5245=CARTESIAN_POINT('Ctrl Pts',(-1.33226797087516,-0.301942438501289,
4.01082320542476));
#5246=CARTESIAN_POINT('Ctrl Pts',(-1.32949625024192,-0.313921782533165,
4.01168277983731));
#5247=CARTESIAN_POINT('Ctrl Pts',(-1.32232457328612,-0.343117242041366,
4.01379711485718));
#5248=CARTESIAN_POINT('Ctrl Pts',(-1.31774978069312,-0.360287637378731,
4.01505725815142));
#5249=CARTESIAN_POINT('Ctrl Pts',(-1.29791964289822,-0.429276419625299,
4.02019057785221));
#5250=CARTESIAN_POINT('Ctrl Pts',(-1.27993361653671,-0.480252292864776,
4.02414773228192));
#5251=CARTESIAN_POINT('Ctrl Pts',(-1.23756794631427,-0.580884491175013,
4.03228539256636));
#5252=CARTESIAN_POINT('Ctrl Pts',(-1.21309480138948,-0.630397992141128,
4.03646159574186));
#5253=CARTESIAN_POINT('Ctrl Pts',(-1.1552666155397,-0.731485057930364,4.04526909171857));
#5254=CARTESIAN_POINT('Ctrl Pts',(-1.1212896358817,-0.782574099851696,4.04989031637467));
#5255=CARTESIAN_POINT('Ctrl Pts',(-1.07488559205689,-0.843090151186601,
4.05545196101681));
#5256=CARTESIAN_POINT('Ctrl Pts',(-1.06558249923752,-0.854818122514659,
4.05653402714784));
#5257=CARTESIAN_POINT('Ctrl Pts',(-1.05103987542027,-0.872544858113575,
4.05817323170261));
#5258=CARTESIAN_POINT('Ctrl Pts',(-1.04593786048779,-0.878654283098264,
4.05873885955268));
#5259=CARTESIAN_POINT('Ctrl Pts',(-1.03684651036115,-0.889349339133849,
4.05972973798537));
#5260=CARTESIAN_POINT('Ctrl Pts',(-1.03287971049476,-0.89395326443013,4.06015647029394));
#5261=CARTESIAN_POINT('Ctrl Pts',(-1.02304723997169,-0.905212146332767,
4.06120072149934));
#5262=CARTESIAN_POINT('Ctrl Pts',(-1.01714726453985,-0.911836683896,4.06181578847821));
#5263=CARTESIAN_POINT('Ctrl Pts',(-0.997408810723819,-0.933569166832068,
4.06383760562203));
#5264=CARTESIAN_POINT('Ctrl Pts',(-0.983294311541937,-0.948424024411138,
4.06522613717319));
#5265=CARTESIAN_POINT('Ctrl Pts',(-0.876599880226736,-1.05577144002512,
4.07536060128387));
#5266=CARTESIAN_POINT('Ctrl Pts',(-0.771485137672042,-1.13485635751599,
4.08345468157651));
#5267=CARTESIAN_POINT('Ctrl Pts',(-0.625335788538119,-1.21498628435347,
4.0944328321397));
#5268=CARTESIAN_POINT('Ctrl Pts',(-0.593296576566292,-1.23094896508899,
4.09681983849976));
#5269=CARTESIAN_POINT('Ctrl Pts',(-0.547487453505306,-1.2515680023658,4.10022969785596));
#5270=CARTESIAN_POINT('Ctrl Pts',(-0.534212316889764,-1.25729159316498,
4.1012174292611));
#5271=CARTESIAN_POINT('Ctrl Pts',(-0.509697032176887,-1.26740303990136,
4.1030422279827));
#5272=CARTESIAN_POINT('Ctrl Pts',(-0.498484684929161,-1.27185476093218,
4.10387709988814));
#5273=CARTESIAN_POINT('Ctrl Pts',(-0.47539943033689,-1.28066831865745,4.10559738510303));
#5274=CARTESIAN_POINT('Ctrl Pts',(-0.463521992871846,-1.28501490415164,
4.10648320225115));
#5275=CARTESIAN_POINT('Ctrl Pts',(-0.433090702643553,-1.29567453579113,
4.10875546596742));
#5276=CARTESIAN_POINT('Ctrl Pts',(-0.414458766812318,-1.30175417014612,
4.1101492517404));
#5277=CARTESIAN_POINT('Ctrl Pts',(-0.311181635169446,-1.33301173992622,
4.11789320099946));
#5278=CARTESIAN_POINT('Ctrl Pts',(-0.224392813245597,-1.35033224301864,
4.12448728392731));
#5279=CARTESIAN_POINT('Ctrl Pts',(-0.0572901278553481,-1.36712115043768,
4.13718131252452));
#5280=CARTESIAN_POINT('Ctrl Pts',(0.0225256901831294,-1.36813630502074,
4.14323785004908));
#5281=CARTESIAN_POINT('Ctrl Pts',(0.116110979418365,-1.3611300623866,4.15007125961564));
#5282=CARTESIAN_POINT('Ctrl Pts',(0.130225441746699,-1.35985226416382,4.151094328248));
#5283=CARTESIAN_POINT('Ctrl Pts',(0.152064817222435,-1.35753194428155,4.15266314069585));
#5284=CARTESIAN_POINT('Ctrl Pts',(0.159804554870582,-1.35664262067354,4.15321634615987));
#5285=CARTESIAN_POINT('Ctrl Pts',(0.17428101997003,-1.35485361177475,4.15424535576591));
#5286=CARTESIAN_POINT('Ctrl Pts',(0.181018969914569,-1.35396983645719,4.15472191378779));
#5287=CARTESIAN_POINT('Ctrl Pts',(0.197280538402448,-1.35171334249654,4.15586671028654));
#5288=CARTESIAN_POINT('Ctrl Pts',(0.206796723594013,-1.35029022795657,4.1565322476128));
#5289=CARTESIAN_POINT('Ctrl Pts',(0.241533176060523,-1.34471965338847,4.15894817127509));
#5290=CARTESIAN_POINT('Ctrl Pts',(0.266652311106611,-1.33996491109726,4.16066923086076));
#5291=CARTESIAN_POINT('Ctrl Pts',(0.334021930735694,-1.32524287723734,4.16525061338459));
#5292=CARTESIAN_POINT('Ctrl Pts',(0.375956134820818,-1.31396225799737,4.16806566275548));
#5293=CARTESIAN_POINT('Ctrl Pts',(0.518228708108931,-1.26831915516917,4.17769908236273));
#5294=CARTESIAN_POINT('Ctrl Pts',(0.615049771833946,-1.22429817111525,4.18443135808958));
#5295=CARTESIAN_POINT('Ctrl Pts',(0.723515021132719,-1.15883989587187,4.19295098079844));
#5296=CARTESIAN_POINT('Ctrl Pts',(0.740979438059369,-1.14775140494888,4.19435465476035));
#5297=CARTESIAN_POINT('Ctrl Pts',(0.768886699671401,-1.12913009517841,4.19665443727495));
#5298=CARTESIAN_POINT('Ctrl Pts',(0.779487027569744,-1.12183843900621,4.19754172383603));
#5299=CARTESIAN_POINT('Ctrl Pts',(0.799842332619613,-1.10740882835426,4.1992733911417));
#5300=CARTESIAN_POINT('Ctrl Pts',(0.809608702437597,-1.10028896321933,4.20011703656367));
#5301=CARTESIAN_POINT('Ctrl Pts',(0.832518821891377,-1.08311688377658,4.20212744739932));
#5302=CARTESIAN_POINT('Ctrl Pts',(0.845576659062321,-1.07295379384322,4.20329838114384));
#5303=CARTESIAN_POINT('Ctrl Pts',(0.89159447047512,-1.03577570720895,4.20751782670116));
#5304=CARTESIAN_POINT('Ctrl Pts',(0.923467989486754,-1.0074612709108,4.21061621933805));
#5305=CARTESIAN_POINT('Ctrl Pts',(1.00364148205996,-0.929234718765019,4.21889002510683));
#5306=CARTESIAN_POINT('Ctrl Pts',(1.04954908381356,-0.8770510708807,4.22413894089452));
#5307=CARTESIAN_POINT('Ctrl Pts',(1.12818525910111,-0.772604040496414,4.23402649902302));
#5308=CARTESIAN_POINT('Ctrl Pts',(1.16174177587119,-0.721163197076716,4.23865258277058));
#5309=CARTESIAN_POINT('Ctrl Pts',(1.19904670025467,-0.654574055545382,4.24421917564556));
#5310=CARTESIAN_POINT('Ctrl Pts',(1.20614980368215,-0.641391363306888,4.24530159923716));
#5311=CARTESIAN_POINT('Ctrl Pts',(1.21669522150949,-0.621025042319853,4.24694122914452));
#5312=CARTESIAN_POINT('Ctrl Pts',(1.22029363380583,-0.613924116314866,4.24750693127685));
#5313=CARTESIAN_POINT('Ctrl Pts',(1.22652938879071,-0.601347311882647,4.24849787318347));
#5314=CARTESIAN_POINT('Ctrl Pts',(1.22919245614337,-0.59588492102953,4.2489245957329));
#5315=CARTESIAN_POINT('Ctrl Pts',(1.23565244683517,-0.582406807658691,4.2499687368707));
#5316=CARTESIAN_POINT('Ctrl Pts',(1.23940789998477,-0.574371593312753,4.25058370492795));
#5317=CARTESIAN_POINT('Ctrl Pts',(1.25157455093782,-0.547664586248167,4.2526048117014));
#5318=CARTESIAN_POINT('Ctrl Pts',(1.25964457183646,-0.528839310491383,4.25399274934889));
#5319=CARTESIAN_POINT('Ctrl Pts',(1.31611456944933,-0.388473703458829,4.26412387237895));
#5320=CARTESIAN_POINT('Ctrl Pts',(1.34725804255815,-0.260715801187346,4.27221545571499));
#5321=CARTESIAN_POINT('Ctrl Pts',(1.36317677128747,-0.094807217177443,4.28319289038459));
#5322=CARTESIAN_POINT('Ctrl Pts',(1.36519394558755,-0.0590294077737234,
4.28558242098447));
#5323=CARTESIAN_POINT('Ctrl Pts',(1.36604848992067,-0.00875608421296452,
4.28899527744985));
#5324=CARTESIAN_POINT('Ctrl Pts',(1.36606462453103,0.00570621309900732,
4.2899833963028));
#5325=CARTESIAN_POINT('Ctrl Pts',(1.36567303550315,0.0322292269052108,4.29180867283752));
#5326=CARTESIAN_POINT('Ctrl Pts',(1.3653351149267,0.0442896236608912,4.29264363055542));
#5327=CARTESIAN_POINT('Ctrl Pts',(1.36431591388661,0.0689781939574303,4.29436383860246));
#5328=CARTESIAN_POINT('Ctrl Pts',(1.36361893096982,0.0816045110707339,4.29524948977124));
#5329=CARTESIAN_POINT('Ctrl Pts',(1.36139583676563,0.113758488019315,4.29752077615866));
#5330=CARTESIAN_POINT('Ctrl Pts',(1.35962487060949,0.133265744908264,4.29891373796646));
#5331=CARTESIAN_POINT('Ctrl Pts',(1.3476311098609,0.239865880797861,4.30661224723844));
#5332=CARTESIAN_POINT('Ctrl Pts',(1.32946098069089,0.325843267923269,4.31315797790196));
#5333=CARTESIAN_POINT('Ctrl Pts',(1.27907901323818,0.48618851179931,4.32586062198181));
#5334=CARTESIAN_POINT('Ctrl Pts',(1.24824531601337,0.560631785938357,4.33197600490831));
#5335=CARTESIAN_POINT('Ctrl Pts',(1.20451205171405,0.644442211880982,4.3388585840369));
#5336=CARTESIAN_POINT('Ctrl Pts',(1.19779155385011,0.656848901940175,4.33987705308452));
#5337=CARTESIAN_POINT('Ctrl Pts',(1.18707010329398,0.675929767431114,4.3414403620864));
#5338=CARTESIAN_POINT('Ctrl Pts',(1.18320254032671,0.682677256663986,4.34199258581071));
#5339=CARTESIAN_POINT('Ctrl Pts',(1.17584584913866,0.695261657938206,4.34302086189557));
#5340=CARTESIAN_POINT('Ctrl Pts',(1.17237060851043,0.701105835417373,4.34349765333229));
#5341=CARTESIAN_POINT('Ctrl Pts',(1.16385885780103,0.715179443591657,4.34464447462523));
#5342=CARTESIAN_POINT('Ctrl Pts',(1.15877855705498,0.723381881663049,4.34531177740591));
#5343=CARTESIAN_POINT('Ctrl Pts',(1.13981904443955,0.753280738179314,4.34774280108668));
#5344=CARTESIAN_POINT('Ctrl Pts',(1.12541304933812,0.774638621350271,4.34947671407069));
#5345=CARTESIAN_POINT('Ctrl Pts',(1.08482019028821,0.831295226687552,4.35410585305907));
#5346=CARTESIAN_POINT('Ctrl Pts',(1.05751955571855,0.865759491866431,4.35695464627477));
#5347=CARTESIAN_POINT('Ctrl Pts',(0.959568696447125,0.977850070039799,4.36654980763222));
#5348=CARTESIAN_POINT('Ctrl Pts',(0.881670374969121,1.04862669573488,4.37321611636102));
#5349=CARTESIAN_POINT('Ctrl Pts',(0.779514351489243,1.1219392004832,4.38166987475214));
#5350=CARTESIAN_POINT('Ctrl Pts',(0.762310351224321,1.13369883378771,4.38308355304672));
#5351=CARTESIAN_POINT('Ctrl Pts',(0.734034310397959,1.15209198822856,4.38539552463061));
#5352=CARTESIAN_POINT('Ctrl Pts',(0.723125057876148,1.15897042642793,4.38628481393576));
#5353=CARTESIAN_POINT('Ctrl Pts',(0.701817996184934,1.17198688120895,4.38801749737081));
#5354=CARTESIAN_POINT('Ctrl Pts',(0.691432946879422,1.17814354515878,4.38886011888069));
#5355=CARTESIAN_POINT('Ctrl Pts',(0.666698304548748,1.1923675318315,4.39086337199337));
#5356=CARTESIAN_POINT('Ctrl Pts',(0.652282082227506,1.20031454355063,4.39202808963276));
#5357=CARTESIAN_POINT('Ctrl Pts',(0.600633365409873,1.22758091639615,4.39619284684034));
#5358=CARTESIAN_POINT('Ctrl Pts',(0.562661944173404,1.2454421852721,4.39924103792595));
#5359=CARTESIAN_POINT('Ctrl Pts',(0.457335927424326,1.28918576809465,4.40765998120004));
#5360=CARTESIAN_POINT('Ctrl Pts',(0.388658927051677,1.31152530517119,4.41311669140555));
#5361=CARTESIAN_POINT('Ctrl Pts',(0.260491452627298,1.34226095313113,4.42308277970975));
#5362=CARTESIAN_POINT('Ctrl Pts',(0.201580359965802,1.35236344734108,4.4275809784457));
#5363=CARTESIAN_POINT('Ctrl Pts',(0.127407832465253,1.36012654905985,4.43301887215503));
#5364=CARTESIAN_POINT('Ctrl Pts',(0.112597970738322,1.36143260118678,4.43409335975041));
#5365=CARTESIAN_POINT('Ctrl Pts',(0.089851605907968,1.36306481755312,4.43572354309389));
#5366=CARTESIAN_POINT('Ctrl Pts',(0.0819291543940543,1.36356394408213,4.4362875932505));
#5367=CARTESIAN_POINT('Ctrl Pts',(0.0679306487509348,1.36432342335475,4.43727713033702));
#5368=CARTESIAN_POINT('Ctrl Pts',(0.0618568013477766,1.36461229471382,4.43770407668093));
#5369=CARTESIAN_POINT('Ctrl Pts',(0.0468862263853533,1.3652241311892,4.43875069555247));
#5370=CARTESIAN_POINT('Ctrl Pts',(0.037987948687809,1.3655007042268,4.43936788638673));
#5371=CARTESIAN_POINT('Ctrl Pts',(0.00841043820728597,1.36613066398238,
4.44140500672592));
#5372=CARTESIAN_POINT('Ctrl Pts',(-0.0122751152794063,1.36610144539997,
4.44280633752552));
#5373=CARTESIAN_POINT('Ctrl Pts',(-0.149420423080392,1.36279199421416,4.45198922257088));
#5374=CARTESIAN_POINT('Ctrl Pts',(-0.265059500413666,1.34509395819356,4.45925235748743));
#5375=CARTESIAN_POINT('Ctrl Pts',(-0.421788411532173,1.30008320556919,4.46989309372466));
#5376=CARTESIAN_POINT('Ctrl Pts',(-0.465828815595272,1.28496095307328,4.47297151842012));
#5377=CARTESIAN_POINT('Ctrl Pts',(-0.525149531164257,1.26114095259945,4.47729747267074));
#5378=CARTESIAN_POINT('Ctrl Pts',(-0.541164425535938,1.25435224364979,4.47848379093162));
#5379=CARTESIAN_POINT('Ctrl Pts',(-0.568098959237523,1.24232288146415,4.48051299900679));
#5380=CARTESIAN_POINT('Ctrl Pts',(-0.579086729531297,1.23723931099467,4.48135059150779));
#5381=CARTESIAN_POINT('Ctrl Pts',(-0.601351810287833,1.22657664785702,4.48306872622031));
#5382=CARTESIAN_POINT('Ctrl Pts',(-0.612622482326328,1.22098646521938,4.48394958083021));
#5383=CARTESIAN_POINT('Ctrl Pts',(-0.640947999549338,1.20644626604826,4.48619255147265));
#5384=CARTESIAN_POINT('Ctrl Pts',(-0.657893243334904,1.19729000011331,4.48756163151049));
#5385=CARTESIAN_POINT('Ctrl Pts',(-0.744640290155184,1.14801913340153,4.49471686268128));
#5386=CARTESIAN_POINT('Ctrl Pts',(-0.81097874001437,1.10215545805635,4.50070269730499));
#5387=CARTESIAN_POINT('Ctrl Pts',(-0.941878575716297,0.993411325213874,
4.51354366854659));
#5388=CARTESIAN_POINT('Ctrl Pts',(-1.00506352597523,0.929435721929034,4.52039034639818));
#5389=CARTESIAN_POINT('Ctrl Pts',(-1.06998902575566,0.849270525263961,4.52788787332642));
#5390=CARTESIAN_POINT('Ctrl Pts',(-1.07830052519696,0.838692406213547,4.52885742704271));
#5391=CARTESIAN_POINT('Ctrl Pts',(-1.09103634361399,0.821981038774539,4.53035645456811));
#5392=CARTESIAN_POINT('Ctrl Pts',(-1.09556805955199,0.815931225706072,4.5308925981133));
#5393=CARTESIAN_POINT('Ctrl Pts',(-1.10412681442433,0.804305462522289,4.53191001305469));
#5394=CARTESIAN_POINT('Ctrl Pts',(-1.1081622931715,0.798736272841784,4.53239179163914));
#5395=CARTESIAN_POINT('Ctrl Pts',(-1.11804235823733,0.784882205189369,4.53357704599625));
#5396=CARTESIAN_POINT('Ctrl Pts',(-1.12383723666935,0.77656208502808,4.53427732343826));
#5397=CARTESIAN_POINT('Ctrl Pts',(-1.13559197330244,0.759277761591802,4.53571023136447));
#5398=CARTESIAN_POINT('Ctrl Pts',(-1.14153919825758,0.750306666325287,4.53644209887711));
#5399=CARTESIAN_POINT('Ctrl Pts',(-1.1473796037955,0.741266514011044,4.53716884124631));
#5400=CARTESIAN_POINT('Origin',(0.,0.,-1.10921167016993));
#5401=CARTESIAN_POINT('',(-1.14737960281818,0.741266515523794,5.25438358752252));
#5402=CARTESIAN_POINT('',(-1.14737960694915,0.741266509129621,5.1349525893656));
#5403=CARTESIAN_POINT('',(-1.14737960344596,0.741266514552077,-1.10921167016993));
#5404=CARTESIAN_POINT('Ctrl Pts',(-1.14737960281818,0.741266515523794,5.25438358752252));
#5405=CARTESIAN_POINT('Ctrl Pts',(-1.11669783189643,0.788757717941165,5.25074885766899));
#5406=CARTESIAN_POINT('Ctrl Pts',(-1.08309694827719,0.834298411855299,5.24710992600634));
#5407=CARTESIAN_POINT('Ctrl Pts',(-1.02265084444286,0.906394317234178,5.24091871128984));
#5408=CARTESIAN_POINT('Ctrl Pts',(-0.99735702289175,0.93415415737226,5.2384156416747));
#5409=CARTESIAN_POINT('Ctrl Pts',(-0.959795903514824,0.972110825285475,
5.23478932399632));
#5410=CARTESIAN_POINT('Ctrl Pts',(-0.94844286229019,0.983190589251895,5.23370425550666));
#5411=CARTESIAN_POINT('Ctrl Pts',(-0.928174891064889,1.00229292962259,5.23178424832833));
#5412=CARTESIAN_POINT('Ctrl Pts',(-0.919342310852199,1.01040063575267,5.23095300820164));
#5413=CARTESIAN_POINT('Ctrl Pts',(-0.900601853912183,1.02715392355282,5.22919991589171));
#5414=CARTESIAN_POINT('Ctrl Pts',(-0.890673617213158,1.03577476709321,5.22827716916442));
#5415=CARTESIAN_POINT('Ctrl Pts',(-0.86374885996307,1.05848057411455,5.22578963248185));
#5416=CARTESIAN_POINT('Ctrl Pts',(-0.846533431717381,1.07229859069501,5.22421455223892));
#5417=CARTESIAN_POINT('Ctrl Pts',(-0.754408727016371,1.14264133572799,5.21586040770549));
#5418=CARTESIAN_POINT('Ctrl Pts',(-0.674167904635609,1.19174401540275,5.20881082342942));
#5419=CARTESIAN_POINT('Ctrl Pts',(-0.54447193355747,1.2537954204792,5.19793470667421));
#5420=CARTESIAN_POINT('Ctrl Pts',(-0.498247251526451,1.2728718637263,5.19415498689192));
#5421=CARTESIAN_POINT('Ctrl Pts',(-0.424809979657135,1.29856344533606,5.18837950056974));
#5422=CARTESIAN_POINT('Ctrl Pts',(-0.398263698719601,1.30694943024731,5.18633693708558));
#5423=CARTESIAN_POINT('Ctrl Pts',(-0.36193699230684,1.3172152097009,5.18361816673078));
#5424=CARTESIAN_POINT('Ctrl Pts',(-0.352366818568368,1.31980753712752,5.18290900356349));
#5425=CARTESIAN_POINT('Ctrl Pts',(-0.336146530968231,1.32401220260077,5.18171995093608));
#5426=CARTESIAN_POINT('Ctrl Pts',(-0.329511120636676,1.3256791591172,5.18123717041773));
#5427=CARTESIAN_POINT('Ctrl Pts',(-0.31542480450765,1.32910563703486,5.1802202561575));
#5428=CARTESIAN_POINT('Ctrl Pts',(-0.307971222037272,1.33085248442282,5.17968680206453));
#5429=CARTESIAN_POINT('Ctrl Pts',(-0.286933129785029,1.33559682856605,5.17819310633613));
#5430=CARTESIAN_POINT('Ctrl Pts',(-0.273316526152427,1.33844970895514,5.17724037381275));
#5431=CARTESIAN_POINT('Ctrl Pts',(-0.17554377492028,1.35738013418546,5.17048403636267));
#5432=CARTESIAN_POINT('Ctrl Pts',(-0.0900723148303787,1.36571860927694,
5.16501680550525));
#5433=CARTESIAN_POINT('Ctrl Pts',(0.069163873994095,1.36622844976993,5.15477838860184));
#5434=CARTESIAN_POINT('Ctrl Pts',(0.142593207758472,1.36052545096765,5.15003503863421));
#5435=CARTESIAN_POINT('Ctrl Pts',(0.2395785150999,1.3450529493333,5.14347202242919));
#5436=CARTESIAN_POINT('Ctrl Pts',(0.263843082430402,1.34050438500095,5.14180546955407));
#5437=CARTESIAN_POINT('Ctrl Pts',(0.30133136283804,1.33241969382357,5.13918480419137));
#5438=CARTESIAN_POINT('Ctrl Pts',(0.314648352973924,1.32933788844693,5.13824478290718));
#5439=CARTESIAN_POINT('Ctrl Pts',(0.339460530722377,1.3232021625791,5.13647513132173));
#5440=CARTESIAN_POINT('Ctrl Pts',(0.350966504286508,1.32019692173747,5.1356471083111));
#5441=CARTESIAN_POINT('Ctrl Pts',(0.376843871901683,1.31307583315212,5.13376737725238));
#5442=CARTESIAN_POINT('Ctrl Pts',(0.391189676763702,1.30887358163759,5.13271301264756));
#5443=CARTESIAN_POINT('Ctrl Pts',(0.428650545634914,1.29722947562982,5.12992618604247));
#5444=CARTESIAN_POINT('Ctrl Pts',(0.451640268405269,1.28940549841292,5.12818188995137));
#5445=CARTESIAN_POINT('Ctrl Pts',(0.569595189229001,1.24572093637903,5.11905053530432));
#5446=CARTESIAN_POINT('Ctrl Pts',(0.660544269572202,1.19997271917198,5.11135698716463));
#5447=CARTESIAN_POINT('Ctrl Pts',(0.778298644189569,1.12326877177145,5.10074414472386));
#5448=CARTESIAN_POINT('Ctrl Pts',(0.810098190585007,1.10055566948255,5.09780809501436));
#5449=CARTESIAN_POINT('Ctrl Pts',(0.859727018226621,1.06178965125214,5.09315374805009));
#5450=CARTESIAN_POINT('Ctrl Pts',(0.878183508706765,1.04657617963331,5.09140567685146));
#5451=CARTESIAN_POINT('Ctrl Pts',(0.903322637649673,1.02472068530454,5.08901060687207));
#5452=CARTESIAN_POINT('Ctrl Pts',(0.91034945917417,1.0184832573611,5.08833955765412));
#5453=CARTESIAN_POINT('Ctrl Pts',(0.922326078502919,1.00762909955756,5.08719388000376));
#5454=CARTESIAN_POINT('Ctrl Pts',(0.927306808247947,1.00304730129117,5.08671686696526));
#5455=CARTESIAN_POINT('Ctrl Pts',(0.938040679291453,0.993024859825739,5.08568782528002));
#5456=CARTESIAN_POINT('Ctrl Pts',(0.943780849207455,0.987570961905156,5.08513677498503));
#5457=CARTESIAN_POINT('Ctrl Pts',(0.960087580985714,0.971805434362287,5.083568036596));
#5458=CARTESIAN_POINT('Ctrl Pts',(0.97053518545871,0.961371657132912,5.08255890599368));
#5459=CARTESIAN_POINT('Ctrl Pts',(1.02902642882004,0.901032230064081,5.07687107971903));
#5460=CARTESIAN_POINT('Ctrl Pts',(1.07339349274715,0.847692837852891,5.07240343368985));
#5461=CARTESIAN_POINT('Ctrl Pts',(1.15148061778871,0.73779551892846,5.06373193442103));
#5462=CARTESIAN_POINT('Ctrl Pts',(1.18554071803918,0.68172023464191,5.05953731919391));
#5463=CARTESIAN_POINT('Ctrl Pts',(1.23362097080065,0.587980902608663,5.05261974958516));
#5464=CARTESIAN_POINT('Ctrl Pts',(1.25023760129873,0.551767821897127,5.04996934726706));
#5465=CARTESIAN_POINT('Ctrl Pts',(1.2713476964716,0.49989293685736,5.04616900024867));
#5466=CARTESIAN_POINT('Ctrl Pts',(1.27718069328018,0.484796197455747,5.04506270385184));
#5467=CARTESIAN_POINT('Ctrl Pts',(1.28688085847206,0.458299540607737,5.0431184749969));
#5468=CARTESIAN_POINT('Ctrl Pts',(1.2908681876091,0.446945319877366,5.04228454842588));
#5469=CARTESIAN_POINT('Ctrl Pts',(1.29885268887806,0.423210260469156,5.04053887449667));
#5470=CARTESIAN_POINT('Ctrl Pts',(1.30282402071905,0.410822081073346,5.03962639042171));
#5471=CARTESIAN_POINT('Ctrl Pts',(1.31285363267612,0.377926637400979,5.03719888799635));
#5472=CARTESIAN_POINT('Ctrl Pts',(1.31860814543316,0.357331319107249,5.03567444018403));
#5473=CARTESIAN_POINT('Ctrl Pts',(1.34869626424871,0.238995832071343,5.02688412657336));
#5474=CARTESIAN_POINT('Ctrl Pts',(1.36263946930033,0.138951299367281,5.01929849513842));
#5475=CARTESIAN_POINT('Ctrl Pts',(1.36675518080256,-0.00776457640466963,
5.00819742301721));
#5476=CARTESIAN_POINT('Ctrl Pts',(1.36571529958815,-0.0538717618015524,
5.00471805672353));
#5477=CARTESIAN_POINT('Ctrl Pts',(1.36040814836661,-0.12628927289488,4.99933531663233));
#5478=CARTESIAN_POINT('Ctrl Pts',(1.35769983165907,-0.152678404004389,4.99739142079486));
#5479=CARTESIAN_POINT('Ctrl Pts',(1.35294725947983,-0.188639244133493,4.99478030960976));
#5480=CARTESIAN_POINT('Ctrl Pts',(1.35156639814453,-0.198291040926888,4.99408325902257));
#5481=CARTESIAN_POINT('Ctrl Pts',(1.34904481183697,-0.214663803886214,4.99290813410803));
#5482=CARTESIAN_POINT('Ctrl Pts',(1.34795692694276,-0.221392377077281,4.99242732974284));
#5483=CARTESIAN_POINT('Ctrl Pts',(1.34552766632889,-0.235735156702116,4.9914072366854));
#5484=CARTESIAN_POINT('Ctrl Pts',(1.34417195452254,-0.24334652048537,4.99086871596583));
#5485=CARTESIAN_POINT('Ctrl Pts',(1.34020026008352,-0.264598084813544,4.98937196961392));
#5486=CARTESIAN_POINT('Ctrl Pts',(1.33744069062105,-0.278210926816376,4.98842113214607));
#5487=CARTESIAN_POINT('Ctrl Pts',(1.31648023815659,-0.374074864716769,4.98176601808539));
#5488=CARTESIAN_POINT('Ctrl Pts',(1.29091025608191,-0.45454005070677,4.97638568426065));
#5489=CARTESIAN_POINT('Ctrl Pts',(1.23604905374828,-0.584241770072027,4.96733178624128));
#5490=CARTESIAN_POINT('Ctrl Pts',(1.21079924696213,-0.634917569518465,4.96368897250628));
#5491=CARTESIAN_POINT('Ctrl Pts',(1.16418588006783,-0.715515785714465,4.95755586542614));
#5492=CARTESIAN_POINT('Ctrl Pts',(1.1446285852634,-0.746402468095068,4.95511713763425));
#5493=CARTESIAN_POINT('Ctrl Pts',(1.11492404252442,-0.789396857108036,4.95156709996658));
#5494=CARTESIAN_POINT('Ctrl Pts',(1.10576805862804,-0.802172041913922,4.95049170068267));
#5495=CARTESIAN_POINT('Ctrl Pts',(1.08925383514937,-0.824393945663081,4.94858261777873));
#5496=CARTESIAN_POINT('Ctrl Pts',(1.0819878855033,-0.833907365839652,4.94775249372462));
#5497=CARTESIAN_POINT('Ctrl Pts',(1.0664375130531,-0.853722292942234,4.94599546532073));
#5498=CARTESIAN_POINT('Ctrl Pts',(1.05812674440812,-0.864001443136632,4.94506758982232));
#5499=CARTESIAN_POINT('Ctrl Pts',(1.0353212284044,-0.891385768571927,4.94254995384899));
#5500=CARTESIAN_POINT('Ctrl Pts',(1.02055293725177,-0.908256699236898,4.94094946023481));
#5501=CARTESIAN_POINT('Ctrl Pts',(0.94747747958175,-0.987702953366598,4.93316514330796));
#5502=CARTESIAN_POINT('Ctrl Pts',(0.883803230494275,-1.04506373427434,4.92676274275056));
#5503=CARTESIAN_POINT('Ctrl Pts',(0.770698991763751,-1.12918305657435,4.91610489898208));
#5504=CARTESIAN_POINT('Ctrl Pts',(0.724225470639474,-1.15953837608525,4.9118998424951));
#5505=CARTESIAN_POINT('Ctrl Pts',(0.650361951015374,-1.20160648791937,4.90557898287706));
#5506=CARTESIAN_POINT('Ctrl Pts',(0.624220346594478,-1.21539214491306,4.90340722042469));
#5507=CARTESIAN_POINT('Ctrl Pts',(0.588552196915119,-1.23274680290621,4.90054860963409));
#5508=CARTESIAN_POINT('Ctrl Pts',(0.579404980237071,-1.23707245265791,4.89982451194704));
#5509=CARTESIAN_POINT('Ctrl Pts',(0.563962784336865,-1.24416608383566,4.89861814065666));
#5510=CARTESIAN_POINT('Ctrl Pts',(0.557693560498852,-1.24698884018793,4.89813277698527));
#5511=CARTESIAN_POINT('Ctrl Pts',(0.544476842621299,-1.25282012950273,4.89711906719937));
#5512=CARTESIAN_POINT('Ctrl Pts',(0.537525244926527,-1.25581842918948,4.89659129886739));
#5513=CARTESIAN_POINT('Ctrl Pts',(0.518107215059327,-1.26400285117295,4.8951311110009));
#5514=CARTESIAN_POINT('Ctrl Pts',(0.505587906529557,-1.26906232995245,4.89420567221588));
#5515=CARTESIAN_POINT('Ctrl Pts',(0.409738729187023,-1.3061546060285,4.88722624374629));
#5516=CARTESIAN_POINT('Ctrl Pts',(0.323512780494029,-1.33013890951881,4.88154203141087));
#5517=CARTESIAN_POINT('Ctrl Pts',(0.155955162309904,-1.35947194658716,4.87060144125238));
#5518=CARTESIAN_POINT('Ctrl Pts',(0.0752875094278573,-1.36631459279741,
4.86537568127857));
#5519=CARTESIAN_POINT('Ctrl Pts',(-0.0247768183454392,-1.36591122005228,
4.85862918802274));
#5520=CARTESIAN_POINT('Ctrl Pts',(-0.0440425062067384,-1.36542577541528,
4.85731884418325));
#5521=CARTESIAN_POINT('Ctrl Pts',(-0.0758624081861914,-1.36394988271716,
4.85513228539503));
#5522=CARTESIAN_POINT('Ctrl Pts',(-0.0884250689942695,-1.36319308115039,
4.85426325994029));
#5523=CARTESIAN_POINT('Ctrl Pts',(-0.113051290509998,-1.36136770957737,
4.85254753091446));
#5524=CARTESIAN_POINT('Ctrl Pts',(-0.125114661858915,-1.3603120743822,4.85170130233038));
#5525=CARTESIAN_POINT('Ctrl Pts',(-0.154468816105163,-1.35734960824288,
4.84962732632031));
#5526=CARTESIAN_POINT('Ctrl Pts',(-0.171739875620201,-1.35527264406935,
4.84839447613882));
#5527=CARTESIAN_POINT('Ctrl Pts',(-0.235037556964589,-1.34643134166058,
4.84382755474198));
#5528=CARTESIAN_POINT('Ctrl Pts',(-0.280745326525242,-1.33764764079029,
4.84043351978184));
#5529=CARTESIAN_POINT('Ctrl Pts',(-0.439087986855978,-1.29874544433809,
4.82834241439823));
#5530=CARTESIAN_POINT('Ctrl Pts',(-0.548229108377538,-1.25657466149148,
4.81935740125709));
#5531=CARTESIAN_POINT('Ctrl Pts',(-0.668872607647689,-1.19121499201174,
4.80925931640299));
#5532=CARTESIAN_POINT('Ctrl Pts',(-0.68683208899175,-1.18095110656499,4.80775297115189));
#5533=CARTESIAN_POINT('Ctrl Pts',(-0.712180473529222,-1.16569045844166,
4.80562934645844));
#5534=CARTESIAN_POINT('Ctrl Pts',(-0.719763462202887,-1.16102361786891,
4.80499439070001));
#5535=CARTESIAN_POINT('Ctrl Pts',(-0.732448992603572,-1.15304443405144,
4.8039334193592));
#5536=CARTESIAN_POINT('Ctrl Pts',(-0.73757582523318,-1.14977167346178,4.80350500180374));
#5537=CARTESIAN_POINT('Ctrl Pts',(-0.749345756293626,-1.14214709995494,
4.80252242096232));
#5538=CARTESIAN_POINT('Ctrl Pts',(-0.755973009903906,-1.13777145185798,
4.8019697957476));
#5539=CARTESIAN_POINT('Ctrl Pts',(-0.77490355692036,-1.12503411045038,4.80039190600163));
#5540=CARTESIAN_POINT('Ctrl Pts',(-0.787109342868636,-1.11652863797659,
4.79937535322496));
#5541=CARTESIAN_POINT('Ctrl Pts',(-0.851424215450019,-1.07013250615786,
4.79400920789582));
#5542=CARTESIAN_POINT('Ctrl Pts',(-0.90094822104981,-1.02878616432678,4.78984026274961));
#5543=CARTESIAN_POINT('Ctrl Pts',(-0.994074530355718,-0.939134799362403,
4.781518703794));
#5544=CARTESIAN_POINT('Ctrl Pts',(-1.03751477248749,-0.890910229189769,
4.77737570281461));
#5545=CARTESIAN_POINT('Ctrl Pts',(-1.1043431998229,-0.80517554617493,4.77026334189846));
#5546=CARTESIAN_POINT('Ctrl Pts',(-1.12963467533398,-0.769289595410338,
4.767352610358));
#5547=CARTESIAN_POINT('Ctrl Pts',(-1.1621089791819,-0.718148867280892,4.76324679818182));
#5548=CARTESIAN_POINT('Ctrl Pts',(-1.17080427200344,-0.703883790771883,
4.76210597745392));
#5549=CARTESIAN_POINT('Ctrl Pts',(-1.1853497715544,-0.679005646001912,4.76012176485244));
#5550=CARTESIAN_POINT('Ctrl Pts',(-1.19132451503696,-0.668467375212106,
4.75928288617851));
#5551=CARTESIAN_POINT('Ctrl Pts',(-1.20333033759404,-0.646619173637664,
4.75754622912605));
#5552=CARTESIAN_POINT('Ctrl Pts',(-1.20934395059617,-0.635301067567886,
4.75664794541302));
#5553=CARTESIAN_POINT('Ctrl Pts',(-1.22452749954289,-0.60572742380612,4.75430338493201));
#5554=CARTESIAN_POINT('Ctrl Pts',(-1.23344845118107,-0.587348403940899,
4.75284882060062));
#5555=CARTESIAN_POINT('Ctrl Pts',(-1.28685982250247,-0.470721978553352,
4.74362912820494));
#5556=CARTESIAN_POINT('Ctrl Pts',(-1.31998812292662,-0.367709640483615,
4.73548724351706));
#5557=CARTESIAN_POINT('Ctrl Pts',(-1.34880897368429,-0.22017632920495,4.72412420243323));
#5558=CARTESIAN_POINT('Ctrl Pts',(-1.35500795093921,-0.178092980712427,
4.72092134630269));
#5559=CARTESIAN_POINT('Ctrl Pts',(-1.36096412204414,-0.118471431837088,
4.71648596875408));
#5560=CARTESIAN_POINT('Ctrl Pts',(-1.36236298952932,-0.101123514533745,
4.71520763174413));
#5561=CARTESIAN_POINT('Ctrl Pts',(-1.36425807572886,-0.0702729931031215,
4.71296095144973));
#5562=CARTESIAN_POINT('Ctrl Pts',(-1.36488620198545,-0.0567809944053895,
4.71198742667749));
#5563=CARTESIAN_POINT('Ctrl Pts',(-1.36555403660669,-0.0357140512168756,
4.71048357585241));
#5564=CARTESIAN_POINT('Ctrl Pts',(-1.36573101351832,-0.0281447347595584,
4.70994651592604));
#5565=CARTESIAN_POINT('Ctrl Pts',(-1.36594741777065,-0.0137783931354472,
4.70893387845222));
#5566=CARTESIAN_POINT('Ctrl Pts',(-1.36599906528825,-0.00698199341434678,
4.70845771493244));
#5567=CARTESIAN_POINT('Ctrl Pts',(-1.36600135147124,0.00986649375045023,
4.70728393151332));
#5568=CARTESIAN_POINT('Ctrl Pts',(-1.36589176392689,0.0199184185880063,
4.7065894763613));
#5569=CARTESIAN_POINT('Ctrl Pts',(-1.36503552898715,0.0589371457037254,
4.703913262923));
#5570=CARTESIAN_POINT('Ctrl Pts',(-1.36347822159935,0.0878805814045542,
4.70196970638826));
#5571=CARTESIAN_POINT('Ctrl Pts',(-1.35642187881346,0.17013577990401,4.69650985455787));
#5572=CARTESIAN_POINT('Ctrl Pts',(-1.34870565060773,0.223204619487589,4.69306256591625));
#5573=CARTESIAN_POINT('Ctrl Pts',(-1.32008737048182,0.362087852607866,4.6839457501852));
#5574=CARTESIAN_POINT('Ctrl Pts',(-1.29395777398044,0.446552875525465,4.67828969535042));
#5575=CARTESIAN_POINT('Ctrl Pts',(-1.25122690709879,0.548532034280309,4.67087464663035));
#5576=CARTESIAN_POINT('Ctrl Pts',(-1.24207913296824,0.568942439811722,4.66936043630902));
#5577=CARTESIAN_POINT('Ctrl Pts',(-1.22673899618773,0.601033996416314,4.66692565248708));
#5578=CARTESIAN_POINT('Ctrl Pts',(-1.22087076822653,0.612866197486269,4.6660159901057));
#5579=CARTESIAN_POINT('Ctrl Pts',(-1.20935715716995,0.6352594976352,4.66427038843218));
#5580=CARTESIAN_POINT('Ctrl Pts',(-1.20374263221296,0.645835135533819,4.66343557453816));
#5581=CARTESIAN_POINT('Ctrl Pts',(-1.19042748359073,0.670138893273853,4.66149206892678));
#5582=CARTESIAN_POINT('Ctrl Pts',(-1.18262728790781,0.68381020109632,4.66037998041908));
#5583=CARTESIAN_POINT('Ctrl Pts',(-1.16579829320398,0.712156670846861,4.65803327081628));
#5584=CARTESIAN_POINT('Ctrl Pts',(-1.15672550157196,0.726800337368898,4.65679734481144));
#5585=CARTESIAN_POINT('Ctrl Pts',(-1.14737959883991,0.741266521681617,4.6555522104354));
#5586=CARTESIAN_POINT('',(-1.3659996708821,-0.000948235195896823,4.5899328338502));
#5587=CARTESIAN_POINT('Ctrl Pts',(-1.1473796037955,0.741266514011044,4.53716884124631));
#5588=CARTESIAN_POINT('Ctrl Pts',(-1.15767679492772,0.72532786460739,4.53845015724928));
#5589=CARTESIAN_POINT('Ctrl Pts',(-1.16764193692774,0.70917455145636,4.53971555061117));
#5590=CARTESIAN_POINT('Ctrl Pts',(-1.21332065966825,0.631555043677277,4.54566613716929));
#5591=CARTESIAN_POINT('Ctrl Pts',(-1.24453852880613,0.567568492559921,4.55019722722848));
#5592=CARTESIAN_POINT('Ctrl Pts',(-1.29621061788948,0.436632580775848,4.55925803753871));
#5593=CARTESIAN_POINT('Ctrl Pts',(-1.31678771034399,0.369971093617939,4.56377370522672));
#5594=CARTESIAN_POINT('Ctrl Pts',(-1.33714275305894,0.280190951277582,4.56994701280096));
#5595=CARTESIAN_POINT('Ctrl Pts',(-1.34155707699873,0.258229019814995,4.57146349227184));
#5596=CARTESIAN_POINT('Ctrl Pts',(-1.34771349509633,0.223156641365741,4.57390088528274));
#5597=CARTESIAN_POINT('Ctrl Pts',(-1.34980871957143,0.210111758630504,4.57481084092691));
#5598=CARTESIAN_POINT('Ctrl Pts',(-1.35337935489555,0.185616704484051,4.57652687584863));
#5599=CARTESIAN_POINT('Ctrl Pts',(-1.35489947434757,0.17417416366768,4.57733149092312));
#5600=CARTESIAN_POINT('Ctrl Pts',(-1.35765762039137,0.151184119954412,4.57895467316746));
#5601=CARTESIAN_POINT('Ctrl Pts',(-1.35889375766979,0.139637362233966,4.57977322779621));
#5602=CARTESIAN_POINT('Ctrl Pts',(-1.36170548673883,0.109780982559263,4.5818988621429));
#5603=CARTESIAN_POINT('Ctrl Pts',(-1.36305903328494,0.0914533261035226,
4.58321254625401));
#5604=CARTESIAN_POINT('Ctrl Pts',(-1.36536424005474,0.0484410470395323,
4.586317372959));
#5605=CARTESIAN_POINT('Ctrl Pts',(-1.36601681405356,0.0237477122534092,
4.58811669886924));
#5606=CARTESIAN_POINT('Ctrl Pts',(-1.3659996708821,-0.000948235195896823,
4.5899328338502));
#5607=CARTESIAN_POINT('Ctrl Pts',(-1.3659996719829,-0.000946648090267182,
4.5899327171348));
#5608=CARTESIAN_POINT('Ctrl Pts',(-1.36595114331841,-0.070972817751537,
4.59508242548681));
#5609=CARTESIAN_POINT('Ctrl Pts',(-1.36051799875388,-0.140887396100429,
4.60036457226783));
#5610=CARTESIAN_POINT('Ctrl Pts',(-1.3388872690427,-0.279868570277552,4.61100460506759));
#5611=CARTESIAN_POINT('Ctrl Pts',(-1.32262581051757,-0.348723951008327,
4.61634601331537));
#5612=CARTESIAN_POINT('Ctrl Pts',(-1.2971544923418,-0.42838632416305,4.62241832949855));
#5613=CARTESIAN_POINT('Ctrl Pts',(-1.2930234244454,-0.440698394500663,4.62335349172859));
#5614=CARTESIAN_POINT('Ctrl Pts',(-1.28624333581331,-0.459988851220078,
4.62481147022928));
#5615=CARTESIAN_POINT('Ctrl Pts',(-1.28371175022734,-0.467007292509119,
4.62534040285606));
#5616=CARTESIAN_POINT('Ctrl Pts',(-1.27874786051624,-0.480423509347495,
4.62634809897938));
#5617=CARTESIAN_POINT('Ctrl Pts',(-1.27632478880541,-0.486824275255625,
4.62682732176821));
#5618=CARTESIAN_POINT('Ctrl Pts',(-1.27012230492207,-0.502844043853325,
4.62802342626027));
#5619=CARTESIAN_POINT('Ctrl Pts',(-1.26628154862607,-0.512439126093901,
4.62873685730318));
#5620=CARTESIAN_POINT('Ctrl Pts',(-1.25122729122657,-0.548844939313722,
4.63143575787438));
#5621=CARTESIAN_POINT('Ctrl Pts',(-1.23926740253139,-0.575340839009211,
4.63338335620342));
#5622=CARTESIAN_POINT('Ctrl Pts',(-1.19339749134004,-0.668880283275949,
4.64026843517801));
#5623=CARTESIAN_POINT('Ctrl Pts',(-1.15481585758506,-0.733485015158952,
4.64504726983616));
#5624=CARTESIAN_POINT('Ctrl Pts',(-1.08290210021077,-0.834045263791338,
4.65301189859273));
#5625=CARTESIAN_POINT('Ctrl Pts',(-1.05260903830645,-0.871964560681386,
4.65615484802548));
#5626=CARTESIAN_POINT('Ctrl Pts',(-0.998314701884474,-0.932965036281039,
4.66155353576328));
#5627=CARTESIAN_POINT('Ctrl Pts',(-0.975370554469441,-0.95692633298336,
4.66377340766147));
#5628=CARTESIAN_POINT('Ctrl Pts',(-0.940681193381317,-0.990608704700189,
4.66706249214752));
#5629=CARTESIAN_POINT('Ctrl Pts',(-0.929608423515292,-1.00100692366398,
4.66810297767876));
#5630=CARTESIAN_POINT('Ctrl Pts',(-0.909548666636262,-1.01922473343583,
4.6699731183939));
#5631=CARTESIAN_POINT('Ctrl Pts',(-0.900628321787931,-1.02711559455379,
4.67079971005194));
#5632=CARTESIAN_POINT('Ctrl Pts',(-0.88137575759624,-1.04370260236612,4.67257384275476));
#5633=CARTESIAN_POINT('Ctrl Pts',(-0.871015536361471,-1.05236412923023,
4.67352265857536));
#5634=CARTESIAN_POINT('Ctrl Pts',(-0.842492168633863,-1.075500964574,4.67612013361844));
#5635=CARTESIAN_POINT('Ctrl Pts',(-0.824086257713378,-1.08966834519801,
4.67778046283123));
#5636=CARTESIAN_POINT('Ctrl Pts',(-0.719909877522258,-1.16570549804802,
4.68709720887509));
#5637=CARTESIAN_POINT('Ctrl Pts',(-0.627551705287686,-1.2179125719106,4.69510174683121));
#5638=CARTESIAN_POINT('Ctrl Pts',(-0.493169615378028,-1.27449878045169,
4.70611676616927));
#5639=CARTESIAN_POINT('Ctrl Pts',(-0.455550096628898,-1.28842457358354,
4.70913269548593));
#5640=CARTESIAN_POINT('Ctrl Pts',(-0.39421812463499,-1.30810523286756,4.7138955944236));
#5641=CARTESIAN_POINT('Ctrl Pts',(-0.370869704899116,-1.31491561132201,
4.71567386331182));
#5642=CARTESIAN_POINT('Ctrl Pts',(-0.33821014330455,-1.32350263183096,4.7181023534611));
#5643=CARTESIAN_POINT('Ctrl Pts',(-0.329044969029845,-1.32581097401784,
4.71877748313826));
#5644=CARTESIAN_POINT('Ctrl Pts',(-0.31327183904545,-1.32960995192767,4.71992762706408));
#5645=CARTESIAN_POINT('Ctrl Pts',(-0.306675577196369,-1.33114686183025,
4.72040508139338));
#5646=CARTESIAN_POINT('Ctrl Pts',(-0.292378482648678,-1.33436612108854,
4.72143211861859));
#5647=CARTESIAN_POINT('Ctrl Pts',(-0.284674151316659,-1.33603097179337,
4.72198076075845));
#5648=CARTESIAN_POINT('Ctrl Pts',(-0.262658774896931,-1.34058924719816,
4.72353598103835));
#5649=CARTESIAN_POINT('Ctrl Pts',(-0.248314691583184,-1.34332014734933,
4.72453422471723));
#5650=CARTESIAN_POINT('Ctrl Pts',(-0.158593510535252,-1.35891537145242,
4.73070016262247));
#5651=CARTESIAN_POINT('Ctrl Pts',(-0.0822819731337005,-1.3656630082639,
4.73560753158714));
#5652=CARTESIAN_POINT('Ctrl Pts',(0.0550589037583409,-1.36624604251924,
4.74443633102323));
#5653=CARTESIAN_POINT('Ctrl Pts',(0.115863559873802,-1.36243707277774,4.74834394047094));
#5654=CARTESIAN_POINT('Ctrl Pts',(0.214065368018784,-1.34966270060912,4.75485663279541));
#5655=CARTESIAN_POINT('Ctrl Pts',(0.251696095409365,-1.34315377305989,4.75740059341008));
#5656=CARTESIAN_POINT('Ctrl Pts',(0.304592678839958,-1.33170332414293,4.7610751249439));
#5657=CARTESIAN_POINT('Ctrl Pts',(0.320121994119462,-1.32805584093332,4.76216603399215));
#5658=CARTESIAN_POINT('Ctrl Pts',(0.347214089329831,-1.32118974371863,4.7640924812776));
#5659=CARTESIAN_POINT('Ctrl Pts',(0.358805155009196,-1.31808907419875,4.764924234507));
#5660=CARTESIAN_POINT('Ctrl Pts',(0.382965202017612,-1.31128384678621,4.76667451195091));
#5661=CARTESIAN_POINT('Ctrl Pts',(0.395524678476943,-1.30755033568398,4.76759388305945));
#5662=CARTESIAN_POINT('Ctrl Pts',(0.428886816590097,-1.29710824763192,4.77006244115314));
#5663=CARTESIAN_POINT('Ctrl Pts',(0.449584677418982,-1.29008031842112,4.77162164754501));
#5664=CARTESIAN_POINT('Ctrl Pts',(0.560555998539736,-1.24940534386587,4.78013720098553));
#5665=CARTESIAN_POINT('Ctrl Pts',(0.647232587107585,-1.20678113303573,4.78738128336765));
#5666=CARTESIAN_POINT('Ctrl Pts',(0.787111503412039,-1.1185624666084,4.79989112826457));
#5667=CARTESIAN_POINT('Ctrl Pts',(0.842659242023877,-1.07733639606051,4.80511122705955));
#5668=CARTESIAN_POINT('Ctrl Pts',(0.904886043370864,-1.02338338160022,4.81109479937021));
#5669=CARTESIAN_POINT('Ctrl Pts',(0.914791137473718,-1.01453906054054,4.81205153111534));
#5670=CARTESIAN_POINT('Ctrl Pts',(0.930103436200013,-1.00045998474769,4.81353526661675));
#5671=CARTESIAN_POINT('Ctrl Pts',(0.935598743359138,-0.995322852870971,
4.81406873164616));
#5672=CARTESIAN_POINT('Ctrl Pts',(0.945990997613875,-0.985445823188159,
4.81507898302722));
#5673=CARTESIAN_POINT('Ctrl Pts',(0.950895316948251,-0.98071429906692,4.8155563010248));
#5674=CARTESIAN_POINT('Ctrl Pts',(0.963028011288096,-0.968832502561183,
4.81673908790891));
#5675=CARTESIAN_POINT('Ctrl Pts',(0.970212533490589,-0.961637678191351,
4.81744127570779));
#5676=CARTESIAN_POINT('Ctrl Pts',(0.996698622197158,-0.934514575267737,
4.8200398234928));
#5677=CARTESIAN_POINT('Ctrl Pts',(1.01547332026404,-0.91407866905551,4.82190183511118));
#5678=CARTESIAN_POINT('Ctrl Pts',(1.08341102262867,-0.835450687671994,4.82878075736254));
#5679=CARTESIAN_POINT('Ctrl Pts',(1.12830406901466,-0.773749891877509,4.83362617620357));
#5680=CARTESIAN_POINT('Ctrl Pts',(1.19318275665264,-0.666829025529125,4.84168211776025));
#5681=CARTESIAN_POINT('Ctrl Pts',(1.21628048201297,-0.623704533628743,4.84484906425385));
#5682=CARTESIAN_POINT('Ctrl Pts',(1.2468431169362,-0.558457658420979,4.84961131698403));
#5683=CARTESIAN_POINT('Ctrl Pts',(1.25613450849916,-0.537232463251863,4.85115586697956));
#5684=CARTESIAN_POINT('Ctrl Pts',(1.2722553348868,-0.497698461355606,4.85403298315287));
#5685=CARTESIAN_POINT('Ctrl Pts',(1.27924035972624,-0.479459522795357,4.85536040943094));
#5686=CARTESIAN_POINT('Ctrl Pts',(1.29009619858651,-0.449185281741076,4.85756749914346));
#5687=CARTESIAN_POINT('Ctrl Pts',(1.2941953523752,-0.437234479901029,4.85843968159622));
#5688=CARTESIAN_POINT('Ctrl Pts',(1.30188595192241,-0.413756810702746,4.86015582246413));
#5689=CARTESIAN_POINT('Ctrl Pts',(1.30549151620741,-0.402235770216086,4.86099923421467));
#5690=CARTESIAN_POINT('Ctrl Pts',(1.31308835291425,-0.37678241166419,4.86286603220854));
#5691=CARTESIAN_POINT('Ctrl Pts',(1.31701150511735,-0.362831469171003,4.86389147901322));
#5692=CARTESIAN_POINT('Ctrl Pts',(1.32991069808374,-0.313992361839857,4.86749047562595));
#5693=CARTESIAN_POINT('Ctrl Pts',(1.33772744184804,-0.278816326032131,4.87009925536449));
#5694=CARTESIAN_POINT('Ctrl Pts',(1.36741811711657,-0.114836764744878,4.88234036029111));
#5695=CARTESIAN_POINT('Ctrl Pts',(1.37213161311019,0.0163524455795227,4.89244283506123));
#5696=CARTESIAN_POINT('Ctrl Pts',(1.35596657487202,0.166517601541037,4.9035542228749));
#5697=CARTESIAN_POINT('Ctrl Pts',(1.35332409044661,0.186781900917488,4.90504194485277));
#5698=CARTESIAN_POINT('Ctrl Pts',(1.34888506692909,0.215739660778059,4.90714431831962));
#5699=CARTESIAN_POINT('Ctrl Pts',(1.34745710748083,0.224485811057334,4.90777619224375));
#5700=CARTESIAN_POINT('Ctrl Pts',(1.34490671272466,0.239204625746198,4.90883364040639));
#5701=CARTESIAN_POINT('Ctrl Pts',(1.34382939566037,0.245184582643006,4.90926157823504));
#5702=CARTESIAN_POINT('Ctrl Pts',(1.34124759166072,0.25898715408451,4.91024533815495));
#5703=CARTESIAN_POINT('Ctrl Pts',(1.3397145368139,0.266804077906842,4.91079959505167));
#5704=CARTESIAN_POINT('Ctrl Pts',(1.33509816314236,0.289298848670706,4.9123874291092));
#5705=CARTESIAN_POINT('Ctrl Pts',(1.33184128227034,0.303940411558971,4.91341212283546));
#5706=CARTESIAN_POINT('Ctrl Pts',(1.31397432640489,0.378450661789922,4.91859545349527));
#5707=CARTESIAN_POINT('Ctrl Pts',(1.29556467300668,0.437341173733927,4.92259030502828));
#5708=CARTESIAN_POINT('Ctrl Pts',(1.25287940455285,0.547182200792347,4.93018118412665));
#5709=CARTESIAN_POINT('Ctrl Pts',(1.22930668083943,0.598264232838212,4.9337743033092));
#5710=CARTESIAN_POINT('Ctrl Pts',(1.17759852575842,0.694269191983003,4.94086231144321));
#5711=CARTESIAN_POINT('Ctrl Pts',(1.1498668453238,0.739292440570475,4.9443440068878));
#5712=CARTESIAN_POINT('Ctrl Pts',(1.10948155411394,0.797068750633401,4.94911169936519));
#5713=CARTESIAN_POINT('Ctrl Pts',(1.0990840263653,0.811345898689302,4.95031571036504));
#5714=CARTESIAN_POINT('Ctrl Pts',(1.08099510709363,0.835198347688162,4.95237429489441));
#5715=CARTESIAN_POINT('Ctrl Pts',(1.07344589569051,0.844879040797041,4.95322339480051));
#5716=CARTESIAN_POINT('Ctrl Pts',(1.05884004467203,0.863096986604661,4.95484823147545));
#5717=CARTESIAN_POINT('Ctrl Pts',(1.0518080078078,0.871652769426327,4.95562295739644));
#5718=CARTESIAN_POINT('Ctrl Pts',(1.03319712006584,0.893743221133499,4.95765453314885));
#5719=CARTESIAN_POINT('Ctrl Pts',(1.02145653679393,0.907138205876561,4.95891778600154));
#5720=CARTESIAN_POINT('Ctrl Pts',(0.975184120298329,0.957893495454662,4.96382984301967));
#5721=CARTESIAN_POINT('Ctrl Pts',(0.938841118700473,0.993539260683248,4.96755176567741));
#5722=CARTESIAN_POINT('Ctrl Pts',(0.832945069684957,1.08639533086097,4.97803011547806));
#5723=CARTESIAN_POINT('Ctrl Pts',(0.759595738793436,1.13888760918944,4.98490770271061));
#5724=CARTESIAN_POINT('Ctrl Pts',(0.649294228475388,1.20239968972569,4.99443298792593));
#5725=CARTESIAN_POINT('Ctrl Pts',(0.616209186307179,1.21968633940467,4.99719368475582));
#5726=CARTESIAN_POINT('Ctrl Pts',(0.572608233220814,1.24023961966086,5.00067522645961));
#5727=CARTESIAN_POINT('Ctrl Pts',(0.562705987928275,1.24476362948729,5.00145577680231));
#5728=CARTESIAN_POINT('Ctrl Pts',(0.546332882281975,1.25200863778534,5.00272858836615));
#5729=CARTESIAN_POINT('Ctrl Pts',(0.539893406529294,1.25479893402066,5.00322470182007));
#5730=CARTESIAN_POINT('Ctrl Pts',(0.526701757224817,1.2603946653866,5.00423150812331));
#5731=CARTESIAN_POINT('Ctrl Pts',(0.519948056032383,1.26319574056828,5.0047419550001));
#5732=CARTESIAN_POINT('Ctrl Pts',(0.501791201565178,1.27055593968199,5.00610173222198));
#5733=CARTESIAN_POINT('Ctrl Pts',(0.490348216875831,1.27501586599862,5.00694556370122));
#5734=CARTESIAN_POINT('Ctrl Pts',(0.415656170956776,1.30297288117292,5.01237833393758));
#5735=CARTESIAN_POINT('Ctrl Pts',(0.350792105499544,1.32191362271648,5.01675119553243));
#5736=CARTESIAN_POINT('Ctrl Pts',(0.216299211381655,1.35058293959469,5.02560741875803));
#5737=CARTESIAN_POINT('Ctrl Pts',(0.146793770598929,1.35989364199503,5.03007773978436));
#5738=CARTESIAN_POINT('Ctrl Pts',(0.0356485690951921,1.36615914636017,5.03737760941438));
#5739=CARTESIAN_POINT('Ctrl Pts',(-0.00566602963778863,1.36661224650933,
5.04012267363819));
#5740=CARTESIAN_POINT('Ctrl Pts',(-0.0633026394535889,1.36463071707727,
5.04403420918818));
#5741=CARTESIAN_POINT('Ctrl Pts',(-0.0796582736774609,1.36377371253939,
5.04515331245001));
#5742=CARTESIAN_POINT('Ctrl Pts',(-0.108024049438008,1.36177540205207,5.04711211071236));
#5743=CARTESIAN_POINT('Ctrl Pts',(-0.120042024082028,1.36076865674156,5.04794761069185));
#5744=CARTESIAN_POINT('Ctrl Pts',(-0.144911672283232,1.35835331415313,5.04968895994036));
#5745=CARTESIAN_POINT('Ctrl Pts',(-0.157759783042428,1.35692112864689,5.05059545423509));
#5746=CARTESIAN_POINT('Ctrl Pts',(-0.191411785425579,1.35268553044258,5.05298876195602));
#5747=CARTESIAN_POINT('Ctrl Pts',(-0.212174046011615,1.34958464115586,5.05448453181308));
#5748=CARTESIAN_POINT('Ctrl Pts',(-0.335123991915285,1.32831462317435,5.0634615162958));
#5749=CARTESIAN_POINT('Ctrl Pts',(-0.435026250830258,1.29902753213487,5.07128628303317));
#5750=CARTESIAN_POINT('Ctrl Pts',(-0.571642103511969,1.24143554984266,5.08249747965414));
#5751=CARTESIAN_POINT('Ctrl Pts',(-0.611787068824816,1.22215134840391,5.08585463934307));
#5752=CARTESIAN_POINT('Ctrl Pts',(-0.673743722892654,1.18857028046148,5.09107553852826));
#5753=CARTESIAN_POINT('Ctrl Pts',(-0.696211296417321,1.17555091423945,5.09297731184821));
#5754=CARTESIAN_POINT('Ctrl Pts',(-0.726524949418517,1.15681074477428,5.09554211102413));
#5755=CARTESIAN_POINT('Ctrl Pts',(-0.734700192448571,1.15163589836958,5.09623368356815));
#5756=CARTESIAN_POINT('Ctrl Pts',(-0.748529401938016,1.14267493948225,5.09740244493148));
#5757=CARTESIAN_POINT('Ctrl Pts',(-0.754211192439227,1.13893273219618,5.09788229219023));
#5758=CARTESIAN_POINT('Ctrl Pts',(-0.766316495362033,1.13082947372757,5.09890364714898));
#5759=CARTESIAN_POINT('Ctrl Pts',(-0.772731124447567,1.12645589638688,5.09944434732102));
#5760=CARTESIAN_POINT('Ctrl Pts',(-0.790645034106759,1.11401692044596,5.1009539391547));
#5761=CARTESIAN_POINT('Ctrl Pts',(-0.80205807828094,1.10582826259066,5.1019152372972));
#5762=CARTESIAN_POINT('Ctrl Pts',(-0.879085964851458,1.04874203299036,5.10841512788209));
#5763=CARTESIAN_POINT('Ctrl Pts',(-0.940326388376973,0.994204067604119,
5.11364974743673));
#5764=CARTESIAN_POINT('Ctrl Pts',(-1.03596822966245,0.892235609094701,5.12263682625932));
#5765=CARTESIAN_POINT('Ctrl Pts',(-1.0728831101018,0.847487938327814,5.12636530671964));
#5766=CARTESIAN_POINT('Ctrl Pts',(-1.12087425100975,0.781133882748675,5.13175664388382));
#5767=CARTESIAN_POINT('Ctrl Pts',(-1.13439091129913,0.761371241133774,5.13334610823854));
#5768=CARTESIAN_POINT('Ctrl Pts',(-1.14737960694915,0.741266509129622,5.1349525893656));
#5769=CARTESIAN_POINT('Origin',(0.,0.,-1.10921167016993));
#5770=CARTESIAN_POINT('',(-1.14737959943097,0.741266520766746,5.85369350940778));
#5771=CARTESIAN_POINT('',(-1.14737961474409,0.741266497064122,5.73596857206561));
#5772=CARTESIAN_POINT('',(-1.14737960344596,0.741266514552077,-1.10921167016993));
#5773=CARTESIAN_POINT('',(-1.36599939927838,0.00101398491177677,5.30997858642083));
#5774=CARTESIAN_POINT('Ctrl Pts',(-1.14737959943097,0.741266520766746,5.85369350940778));
#5775=CARTESIAN_POINT('Ctrl Pts',(-1.12811340835725,0.771087960124151,5.85103670934246));
#5776=CARTESIAN_POINT('Ctrl Pts',(-1.10768818488231,0.80015270559341,5.84840821513957));
#5777=CARTESIAN_POINT('Ctrl Pts',(-1.07904096174742,0.837713551471296,5.84498877000203));
#5778=CARTESIAN_POINT('Ctrl Pts',(-1.07181268446122,0.846942137620228,5.84414675067462));
#5779=CARTESIAN_POINT('Ctrl Pts',(-1.05995852614563,0.86168187722696,5.84280032055335));
#5780=CARTESIAN_POINT('Ctrl Pts',(-1.05540651333128,0.867251308693703,5.84229120035501));
#5781=CARTESIAN_POINT('Ctrl Pts',(-1.04626299955735,0.878259866956038,5.84128456402475));
#5782=CARTESIAN_POINT('Ctrl Pts',(-1.04167257144467,0.883699562818069,5.84078700820547));
#5783=CARTESIAN_POINT('Ctrl Pts',(-1.02964316162297,0.897730526525831,5.83950250054803));
#5784=CARTESIAN_POINT('Ctrl Pts',(-1.0221389317644,0.906265504193979,5.83872002301181));
#5785=CARTESIAN_POINT('Ctrl Pts',(-0.985286874755471,0.947139253643286,
5.83496156000605));
#5786=CARTESIAN_POINT('Ctrl Pts',(-0.954503372171459,0.97815494830725,5.83207469776374));
#5787=CARTESIAN_POINT('Ctrl Pts',(-0.880773689032535,1.04563869717357,5.82556086518511));
#5788=CARTESIAN_POINT('Ctrl Pts',(-0.836954522955105,1.08103195991599,5.82196567300046));
#5789=CARTESIAN_POINT('Ctrl Pts',(-0.730562427260768,1.15660895791635,5.8135622418388));
#5790=CARTESIAN_POINT('Ctrl Pts',(-0.666653002631692,1.19458679309199,5.80874250763971));
#5791=CARTESIAN_POINT('Ctrl Pts',(-0.582733046079055,1.23561594404124,5.80244364628271));
#5792=CARTESIAN_POINT('Ctrl Pts',(-0.565310879736616,1.24368328476196,5.80113808239805));
#5793=CARTESIAN_POINT('Ctrl Pts',(-0.536208454913331,1.25642132184685,5.79895726280657));
#5794=CARTESIAN_POINT('Ctrl Pts',(-0.524623029064137,1.26130278059111,5.7980891152715));
#5795=CARTESIAN_POINT('Ctrl Pts',(-0.501608207704325,1.27062801318209,5.79636365266059));
#5796=CARTESIAN_POINT('Ctrl Pts',(-0.490183068718569,1.27507916765229,5.79550667807287));
#5797=CARTESIAN_POINT('Ctrl Pts',(-0.462251404406642,1.28553026763013,5.79340979770544));
#5798=CARTESIAN_POINT('Ctrl Pts',(-0.445686485640865,1.29136669286971,5.79216472205752));
#5799=CARTESIAN_POINT('Ctrl Pts',(-0.379872986028528,1.3131380917556,5.78720956069329));
#5800=CARTESIAN_POINT('Ctrl Pts',(-0.329853423363826,1.32658610131011,5.78342296374403));
#5801=CARTESIAN_POINT('Ctrl Pts',(-0.193373360763067,1.3550828482592,5.77304821430273));
#5802=CARTESIAN_POINT('Ctrl Pts',(-0.106025444677121,1.3646977095611,5.76635160627938));
#5803=CARTESIAN_POINT('Ctrl Pts',(0.0201150312704392,1.36639400975591,5.75690010543974));
#5804=CARTESIAN_POINT('Ctrl Pts',(0.0586064109977944,1.36528496880573,5.75404822983349));
#5805=CARTESIAN_POINT('Ctrl Pts',(0.108250712098863,1.36175068911321,5.75044971052708));
#5806=CARTESIAN_POINT('Ctrl Pts',(0.11948871820148,1.36081064934967,5.74964045007355));
#5807=CARTESIAN_POINT('Ctrl Pts',(0.137083272822926,1.35911924259943,5.74838310679252));
#5808=CARTESIAN_POINT('Ctrl Pts',(0.14344808135378,1.3584622157274,5.7479302508863));
#5809=CARTESIAN_POINT('Ctrl Pts',(0.156792652316215,1.35698984541692,5.74698527775598));
#5810=CARTESIAN_POINT('Ctrl Pts',(0.163771168280475,1.35616532343295,5.74649372011592));
#5811=CARTESIAN_POINT('Ctrl Pts',(0.18158120642322,1.35392156097395,5.74524519028295));
#5812=CARTESIAN_POINT('Ctrl Pts',(0.192402929915145,1.35242613828876,5.74449222180828));
#5813=CARTESIAN_POINT('Ctrl Pts',(0.240522614915606,1.34518731647118,5.74116466539435));
#5814=CARTESIAN_POINT('Ctrl Pts',(0.277594310465031,1.33802914498583,5.73865615017316));
#5815=CARTESIAN_POINT('Ctrl Pts',(0.404466066749011,1.30803014009805,5.73011646518757));
#5816=CARTESIAN_POINT('Ctrl Pts',(0.492207106888203,1.27760288851509,5.72427505359968));
#5817=CARTESIAN_POINT('Ctrl Pts',(0.619886403456356,1.21820310367045,5.71509735254835));
#5818=CARTESIAN_POINT('Ctrl Pts',(0.662466281805737,1.19558172075626,5.71191394260033));
#5819=CARTESIAN_POINT('Ctrl Pts',(0.718848196878404,1.16168981017179,5.70746409455181));
#5820=CARTESIAN_POINT('Ctrl Pts',(0.733759802198443,1.15232914156233,5.70626376684042));
#5821=CARTESIAN_POINT('Ctrl Pts',(0.758646355095302,1.13602783400398,5.70421779487226));
#5822=CARTESIAN_POINT('Ctrl Pts',(0.768717406244891,1.12923738186927,5.70337766227386));
#5823=CARTESIAN_POINT('Ctrl Pts',(0.788993560471834,1.11516915312739,5.70166046108495));
#5824=CARTESIAN_POINT('Ctrl Pts',(0.799191698782948,1.10788342737899,5.70078315249443));
#5825=CARTESIAN_POINT('Ctrl Pts',(0.824598801950516,1.08919879938662,5.6985620235798));
#5826=CARTESIAN_POINT('Ctrl Pts',(0.839672373258382,1.07762119965418,5.69721151907929));
#5827=CARTESIAN_POINT('Ctrl Pts',(0.911450161597383,1.02007018549913,5.69061618078121));
#5828=CARTESIAN_POINT('Ctrl Pts',(0.964640752949628,0.96992256760908,5.68520996884125));
#5829=CARTESIAN_POINT('Ctrl Pts',(1.06442425962048,0.859483760170551,5.67400587012014));
#5830=CARTESIAN_POINT('Ctrl Pts',(1.11050640986662,0.799053935867799,5.6682202998947));
#5831=CARTESIAN_POINT('Ctrl Pts',(1.16647052175749,0.711402622186961,5.66049443552602));
#5832=CARTESIAN_POINT('Ctrl Pts',(1.18087277856443,0.687231329839464,5.65842816478654));
#5833=CARTESIAN_POINT('Ctrl Pts',(1.19947620653614,0.653695071007281,5.65566351393403));
#5834=CARTESIAN_POINT('Ctrl Pts',(1.20433281079463,0.644703740383673,5.65493202002744));
#5835=CARTESIAN_POINT('Ctrl Pts',(1.21226395527527,0.629617880907142,5.65372185512977));
#5836=CARTESIAN_POINT('Ctrl Pts',(1.21539447739533,0.623553402611398,5.65323994074028));
#5837=CARTESIAN_POINT('Ctrl Pts',(1.221872440534,0.61077006971569,5.65223399826883));
#5838=CARTESIAN_POINT('Ctrl Pts',(1.22521016544028,0.604046683897153,5.65171053597974));
#5839=CARTESIAN_POINT('Ctrl Pts',(1.23426188914298,0.585429490421958,5.650275532307));
#5840=CARTESIAN_POINT('Ctrl Pts',(1.23985941064889,0.573479531817133,5.64937058595956));
#5841=CARTESIAN_POINT('Ctrl Pts',(1.25221819251087,0.54606802855242,5.64732710258067));
#5842=CARTESIAN_POINT('Ctrl Pts',(1.25886797606314,0.530558353341643,5.6461939233601));
#5843=CARTESIAN_POINT('Ctrl Pts',(1.28044360758679,0.477544969917856,5.64238518879082));
#5844=CARTESIAN_POINT('Ctrl Pts',(1.29399491468335,0.439502695973512,5.63975976881507));
#5845=CARTESIAN_POINT('Ctrl Pts',(1.33721109196928,0.298740506565782,5.6302509688775));
#5846=CARTESIAN_POINT('Ctrl Pts',(1.35647811827134,0.1932479909177,5.62348217538948));
#5847=CARTESIAN_POINT('Ctrl Pts',(1.36468783518042,0.0639971828951293,5.61480067335884));
#5848=CARTESIAN_POINT('Ctrl Pts',(1.36556096056847,0.0413726154390076,5.61326840234323));
#5849=CARTESIAN_POINT('Ctrl Pts',(1.36605340070809,0.00547676935262888,
5.61081157977231));
#5850=CARTESIAN_POINT('Ctrl Pts',(1.36604218403481,-0.00778581354329597,
5.6098982983631));
#5851=CARTESIAN_POINT('Ctrl Pts',(1.3656536071336,-0.0330038856479323,5.60815012901416));
#5852=CARTESIAN_POINT('Ctrl Pts',(1.36531231819664,-0.0449587471834363,
5.60731642664285));
#5853=CARTESIAN_POINT('Ctrl Pts',(1.36416303783,-0.0725220855555203,5.60538202811318));
#5854=CARTESIAN_POINT('Ctrl Pts',(1.36324406248576,-0.0881239853978485,
5.60427803944421));
#5855=CARTESIAN_POINT('Ctrl Pts',(1.35932782890157,-0.139559094175983,5.60060697649554));
#5856=CARTESIAN_POINT('Ctrl Pts',(1.35518371153783,-0.175287134731346,5.59800587615646));
#5857=CARTESIAN_POINT('Ctrl Pts',(1.34113443382196,-0.265233713003493,5.59132512831303));
#5858=CARTESIAN_POINT('Ctrl Pts',(1.32934959755508,-0.319091086169834,5.5871996621979));
#5859=CARTESIAN_POINT('Ctrl Pts',(1.29063415975088,-0.455848726721799,5.57646944920219));
#5860=CARTESIAN_POINT('Ctrl Pts',(1.25896676498579,-0.537158615925589,5.56983106015817));
#5861=CARTESIAN_POINT('Ctrl Pts',(1.21357863623652,-0.627193969891007,5.56249802814622));
#5862=CARTESIAN_POINT('Ctrl Pts',(1.20719818571257,-0.639388738890343,5.56150556857924));
#5863=CARTESIAN_POINT('Ctrl Pts',(1.19699799102136,-0.658186857115488,5.5599791744674));
#5864=CARTESIAN_POINT('Ctrl Pts',(1.19330560205386,-0.66485778679711,5.55943819222689));
#5865=CARTESIAN_POINT('Ctrl Pts',(1.18618858797609,-0.677465570299977,5.55841756943209));
#5866=CARTESIAN_POINT('Ctrl Pts',(1.18277487450405,-0.683408050539663,5.55793734762481));
#5867=CARTESIAN_POINT('Ctrl Pts',(1.17427735270562,-0.69794585458701,5.55676405847408));
#5868=CARTESIAN_POINT('Ctrl Pts',(1.16914362488872,-0.706511794908748,5.5560740356382));
#5869=CARTESIAN_POINT('Ctrl Pts',(1.14904038219926,-0.739235995949547,5.55343990553807));
#5870=CARTESIAN_POINT('Ctrl Pts',(1.13341124766477,-0.762982871582658,5.55153248002844));
#5871=CARTESIAN_POINT('Ctrl Pts',(1.08723990934802,-0.828581966910275,5.54622354522196));
#5872=CARTESIAN_POINT('Ctrl Pts',(1.05504162121242,-0.869210313240072,5.5428866022548));
#5873=CARTESIAN_POINT('Ctrl Pts',(0.960193589929525,-0.975831662356207,
5.53370959418636));
#5874=CARTESIAN_POINT('Ctrl Pts',(0.893153656820455,-1.03754208210594,5.52789037941165));
#5875=CARTESIAN_POINT('Ctrl Pts',(0.802689002983414,-1.10550524574623,5.52030103713272));
#5876=CARTESIAN_POINT('Ctrl Pts',(0.784569004379448,-1.11843769123451,5.51879372696432));
#5877=CARTESIAN_POINT('Ctrl Pts',(0.755225044619035,-1.13831674253875,5.5163673597787));
#5878=CARTESIAN_POINT('Ctrl Pts',(0.744201969236459,-1.14555370129841,5.51545907792456));
#5879=CARTESIAN_POINT('Ctrl Pts',(0.722968187949847,-1.15905845366703,5.51371442503807));
#5880=CARTESIAN_POINT('Ctrl Pts',(0.712776364461891,-1.16535373943174,5.51287915614465));
#5881=CARTESIAN_POINT('Ctrl Pts',(0.688967071333869,-1.17963108315959,5.51093202598312));
#5882=CARTESIAN_POINT('Ctrl Pts',(0.675291659330994,-1.18751263384023,5.5098167265655));
#5883=CARTESIAN_POINT('Ctrl Pts',(0.629113799296732,-1.21307072154672,5.50605918041482));
#5884=CARTESIAN_POINT('Ctrl Pts',(0.59603281852178,-1.22966222034964,5.50338062668796));
#5885=CARTESIAN_POINT('Ctrl Pts',(0.50971590974709,-1.26865193555939,5.49642247401979));
#5886=CARTESIAN_POINT('Ctrl Pts',(0.455661276352021,-1.28905380745921,5.49209169331816));
#5887=CARTESIAN_POINT('Ctrl Pts',(0.321881874064552,-1.33007789978373,5.48151917735493));
#5888=CARTESIAN_POINT('Ctrl Pts',(0.241259433426665,-1.34703788201261,5.4752620821045));
#5889=CARTESIAN_POINT('Ctrl Pts',(0.145664043116108,-1.35828376228655,5.4682554512615));
#5890=CARTESIAN_POINT('Ctrl Pts',(0.13170673047209,-1.35970811873738,5.46724290876802));
#5891=CARTESIAN_POINT('Ctrl Pts',(0.109997125192415,-1.36158615818662,5.4656865992969));
#5892=CARTESIAN_POINT('Ctrl Pts',(0.102259161179741,-1.36218915911001,5.46513554955022));
#5893=CARTESIAN_POINT('Ctrl Pts',(0.0877257108335951,-1.36319717310451,
5.46410795574094));
#5894=CARTESIAN_POINT('Ctrl Pts',(0.0809320141986718,-1.36361737462213,
5.46363069247365));
#5895=CARTESIAN_POINT('Ctrl Pts',(0.0644618052833058,-1.36451255897796,
5.462480680883));
#5896=CARTESIAN_POINT('Ctrl Pts',(0.0547828935567366,-1.36493541835123,
5.46181069777981));
#5897=CARTESIAN_POINT('Ctrl Pts',(0.0190694938133556,-1.36611517761471,
5.45935738793531));
#5898=CARTESIAN_POINT('Ctrl Pts',(-0.00698225003111828,-1.36623049999388,
5.45760458150581));
#5899=CARTESIAN_POINT('Ctrl Pts',(-0.0777504449832397,-1.36451916767586,
5.45290486302397));
#5900=CARTESIAN_POINT('Ctrl Pts',(-0.122400546815885,-1.36124072985494,
5.450006118593));
#5901=CARTESIAN_POINT('Ctrl Pts',(-0.26934852992166,-1.34316056719411,5.44046590734403));
#5902=CARTESIAN_POINT('Ctrl Pts',(-0.370112591271138,-1.31895540498923,
5.43389606617279));
#5903=CARTESIAN_POINT('Ctrl Pts',(-0.486966884504906,-1.27642568474055,
5.42553864069193));
#5904=CARTESIAN_POINT('Ctrl Pts',(-0.506581308770287,-1.26876892071136,
5.42411067722837));
#5905=CARTESIAN_POINT('Ctrl Pts',(-0.537954635311713,-1.2556784303353,5.42178113253919));
#5906=CARTESIAN_POINT('Ctrl Pts',(-0.54982734971787,-1.25052523998784,5.42088881570568));
#5907=CARTESIAN_POINT('Ctrl Pts',(-0.572617020700198,-1.24024641057731,
5.41915416238086));
#5908=CARTESIAN_POINT('Ctrl Pts',(-0.583542879392435,-1.23514335315846,
5.41831264998797));
#5909=CARTESIAN_POINT('Ctrl Pts',(-0.609122052391537,-1.22278113668598,
5.41631835679555));
#5910=CARTESIAN_POINT('Ctrl Pts',(-0.623715115103117,-1.21540231897139,
5.41516159701297));
#5911=CARTESIAN_POINT('Ctrl Pts',(-0.674497387262082,-1.18856941308465,
5.41106695761327));
#5912=CARTESIAN_POINT('Ctrl Pts',(-0.709935049411847,-1.1677480858733,5.40808310346114));
#5913=CARTESIAN_POINT('Ctrl Pts',(-0.802522777739353,-1.10757483865519,
5.39993823675457));
#5914=CARTESIAN_POINT('Ctrl Pts',(-0.857701131903669,-1.06541635086511,
5.39469869524285));
#5915=CARTESIAN_POINT('Ctrl Pts',(-0.960434113196507,-0.973752402194657,
5.38428458147063));
#5916=CARTESIAN_POINT('Ctrl Pts',(-1.00795079010317,-0.924480667589373,
5.3791255862122));
#5917=CARTESIAN_POINT('Ctrl Pts',(-1.05945319542635,-0.862361284379285,
5.37327578903984));
#5918=CARTESIAN_POINT('Ctrl Pts',(-1.06719507006544,-0.852761846993567,
5.37238885976758));
#5919=CARTESIAN_POINT('Ctrl Pts',(-1.07932595386523,-0.83729631295194,5.37098852001014));
#5920=CARTESIAN_POINT('Ctrl Pts',(-1.08379940883366,-0.831497731931924,
5.37046973924917));
#5921=CARTESIAN_POINT('Ctrl Pts',(-1.09246490760222,-0.820076584204894,
5.36946054683667));
#5922=CARTESIAN_POINT('Ctrl Pts',(-1.09666065197684,-0.814457240238254,
5.36896991996012));
#5923=CARTESIAN_POINT('Ctrl Pts',(-1.10723959764355,-0.800058923374119,
5.36772707626161));
#5924=CARTESIAN_POINT('Ctrl Pts',(-1.11356195672795,-0.791235486326229,
5.36697879007257));
#5925=CARTESIAN_POINT('Ctrl Pts',(-1.14092055316001,-0.752076449634641,
5.36371151721501));
#5926=CARTESIAN_POINT('Ctrl Pts',(-1.16082911439143,-0.720968085848893,
5.36125567827709));
#5927=CARTESIAN_POINT('Ctrl Pts',(-1.20607386929054,-0.643526464700441,
5.35537606041516));
#5928=CARTESIAN_POINT('Ctrl Pts',(-1.23003197699511,-0.5964581567411,5.3519933548579));
#5929=CARTESIAN_POINT('Ctrl Pts',(-1.28275353915265,-0.476109263892447,
5.34354642634669));
#5930=CARTESIAN_POINT('Ctrl Pts',(-1.30802089038347,-0.4015173995275,5.33847916256507));
#5931=CARTESIAN_POINT('Ctrl Pts',(-1.33215155124514,-0.303061769322372,
5.33168540456953));
#5932=CARTESIAN_POINT('Ctrl Pts',(-1.33701660729152,-0.280821447301688,
5.33014492999682));
#5933=CARTESIAN_POINT('Ctrl Pts',(-1.34383773284858,-0.245423521469275,
5.32767808412711));
#5934=CARTESIAN_POINT('Ctrl Pts',(-1.34616136843354,-0.232340495840752,
5.32676314723762));
#5935=CARTESIAN_POINT('Ctrl Pts',(-1.35015251861225,-0.207793946913368,
5.32503951435536));
#5936=CARTESIAN_POINT('Ctrl Pts',(-1.35186579661275,-0.196338995950011,
5.32423232006003));
#5937=CARTESIAN_POINT('Ctrl Pts',(-1.35500114798998,-0.173384338772403,
5.32260852186823));
#5938=CARTESIAN_POINT('Ctrl Pts',(-1.35642297505521,-0.161885570886295,
5.32179198182166));
#5939=CARTESIAN_POINT('Ctrl Pts',(-1.35998783228077,-0.12969838390021,5.3194970049368));
#5940=CARTESIAN_POINT('Ctrl Pts',(-1.36180480488839,-0.108977817475672,
5.31800882229745));
#5941=CARTESIAN_POINT('Ctrl Pts',(-1.36507084082304,-0.0585147998587496,
5.31435673505237));
#5942=CARTESIAN_POINT('Ctrl Pts',(-1.36602175362683,-0.0287522005951587,
5.31217927100926));
#5943=CARTESIAN_POINT('Ctrl Pts',(-1.3659996224837,0.00101556604943034,
5.30997885891414));
#5944=CARTESIAN_POINT('Ctrl Pts',(-1.36599962363692,0.00101401369812244,
5.30997897366282));
#5945=CARTESIAN_POINT('Ctrl Pts',(-1.36591453674133,0.115636397574861,5.30150617172131));
#5946=CARTESIAN_POINT('Ctrl Pts',(-1.35140392567906,0.229783323934746,5.29268365016902));
#5947=CARTESIAN_POINT('Ctrl Pts',(-1.31641703436901,0.365594045425327,5.28229751583335));
#5948=CARTESIAN_POINT('Ctrl Pts',(-1.30932584318178,0.390229226810623,5.280420654698));
#5949=CARTESIAN_POINT('Ctrl Pts',(-1.29862120705221,0.423829850540205,5.27788313415047));
#5950=CARTESIAN_POINT('Ctrl Pts',(-1.29560019362518,0.432976827982795,5.27719468143049));
#5951=CARTESIAN_POINT('Ctrl Pts',(-1.29028227490084,0.448524103978794,5.27602936762576));
#5952=CARTESIAN_POINT('Ctrl Pts',(-1.28803393185139,0.454940457090177,5.27554989070704));
#5953=CARTESIAN_POINT('Ctrl Pts',(-1.28310718714189,0.468671109057133,5.27452718288019));
#5954=CARTESIAN_POINT('Ctrl Pts',(-1.2804140078954,0.47597966142664,5.2739847861442));
#5955=CARTESIAN_POINT('Ctrl Pts',(-1.27264996126539,0.49650628584666,5.27246591749855));
#5956=CARTESIAN_POINT('Ctrl Pts',(-1.26743575630958,0.509669558193727,5.27149718474744));
#5957=CARTESIAN_POINT('Ctrl Pts',(-1.23147895875168,0.596476080521171,5.26512890149727));
#5958=CARTESIAN_POINT('Ctrl Pts',(-1.19453447072306,0.667394026218049,5.26001719739372));
#5959=CARTESIAN_POINT('Ctrl Pts',(-1.15020188489181,0.736884263153701,5.25471866229315));
#5960=CARTESIAN_POINT('Ctrl Pts',(-1.14879384500244,0.739077461247534,5.2545511263618));
#5961=CARTESIAN_POINT('Ctrl Pts',(-1.14737960281818,0.741266515523794,5.25438358752252));
#5962=CARTESIAN_POINT('Ctrl Pts',(-1.14737960694915,0.741266509129622,5.1349525893656));
#5963=CARTESIAN_POINT('Ctrl Pts',(-1.15450894696792,0.730231261687857,5.13583436768247));
#5964=CARTESIAN_POINT('Ctrl Pts',(-1.16147922321502,0.719092948402125,5.13672125066156));
#5965=CARTESIAN_POINT('Ctrl Pts',(-1.17647240150357,0.694347267289952,5.13868640863433));
#5966=CARTESIAN_POINT('Ctrl Pts',(-1.1844214162519,0.680699135474698,5.13976688572985));
#5967=CARTESIAN_POINT('Ctrl Pts',(-1.19797950498453,0.656463683518967,5.14168150157374));
#5968=CARTESIAN_POINT('Ctrl Pts',(-1.20368936084057,0.645934492702167,5.1425120056133));
#5969=CARTESIAN_POINT('Ctrl Pts',(-1.21538765439165,0.62366852794634,5.14426629621625));
#5970=CARTESIAN_POINT('Ctrl Pts',(-1.22134618530777,0.611917524922512,5.14519101030784));
#5971=CARTESIAN_POINT('Ctrl Pts',(-1.2368934577186,0.580124263251856,5.1476908755887));
#5972=CARTESIAN_POINT('Ctrl Pts',(-1.24616438612236,0.559931966528528,5.14927650203044));
#5973=CARTESIAN_POINT('Ctrl Pts',(-1.29893217937928,0.437193445085112,5.15890798489505));
#5974=CARTESIAN_POINT('Ctrl Pts',(-1.33023776296448,0.329881369553427,5.16735092085455));
#5975=CARTESIAN_POINT('Ctrl Pts',(-1.35647845897519,0.169068066811006,5.17965084744787));
#5976=CARTESIAN_POINT('Ctrl Pts',(-1.36189655802888,0.117713919453158,5.18351917466306));
#5977=CARTESIAN_POINT('Ctrl Pts',(-1.36508952614646,0.0518784708489853,
5.18831831453016));
#5978=CARTESIAN_POINT('Ctrl Pts',(-1.36555813590157,0.0375740417395821,
5.18935133300515));
#5979=CARTESIAN_POINT('Ctrl Pts',(-1.36593363012036,0.0155294052801895,
5.19092581799107));
#5980=CARTESIAN_POINT('Ctrl Pts',(-1.36599967616427,0.00779338323103472,
5.19147502449439));
#5981=CARTESIAN_POINT('Ctrl Pts',(-1.36600028311803,-0.00675474728496466,
5.19250109548764));
#5982=CARTESIAN_POINT('Ctrl Pts',(-1.36594961932748,-0.0135660898302727,
5.19297865092577));
#5983=CARTESIAN_POINT('Ctrl Pts',(-1.36570284638087,-0.0301068606673808,
5.19413190119696));
#5984=CARTESIAN_POINT('Ctrl Pts',(-1.36545372279224,-0.0398350662353058,
5.1948047868326));
#5985=CARTESIAN_POINT('Ctrl Pts',(-1.36414327017427,-0.0759306051827434,
5.19728424352104));
#5986=CARTESIAN_POINT('Ctrl Pts',(-1.36242189053262,-0.102269862442182,
5.19905943513985));
#5987=CARTESIAN_POINT('Ctrl Pts',(-1.35563665462605,-0.174054276210706,
5.20384422909637));
#5988=CARTESIAN_POINT('Ctrl Pts',(-1.34905295166681,-0.21932239868494,5.20680351483517));
#5989=CARTESIAN_POINT('Ctrl Pts',(-1.32059528484207,-0.36369216799689,5.21628158880166));
#5990=CARTESIAN_POINT('Ctrl Pts',(-1.28995942306744,-0.460702006339788,
5.22273812161931));
#5991=CARTESIAN_POINT('Ctrl Pts',(-1.24024427337802,-0.572890479318851,
5.23098181524686));
#5992=CARTESIAN_POINT('Ctrl Pts',(-1.23116434737239,-0.592151692939552,
5.23242546088701));
#5993=CARTESIAN_POINT('Ctrl Pts',(-1.21582697051859,-0.622807735452572,
5.23477396790487));
#5994=CARTESIAN_POINT('Ctrl Pts',(-1.20985036748271,-0.634339629824502,
5.2356692715818));
#5995=CARTESIAN_POINT('Ctrl Pts',(-1.19802007244958,-0.65639072506628,5.23740527464382));
#5996=CARTESIAN_POINT('Ctrl Pts',(-1.19218996286681,-0.666921250279914,
5.23824509218044));
#5997=CARTESIAN_POINT('Ctrl Pts',(-1.17817805405076,-0.691459027069183,
5.24022825661707));
#5998=CARTESIAN_POINT('Ctrl Pts',(-1.16988455275361,-0.70540003274223,5.24137545907456));
#5999=CARTESIAN_POINT('Ctrl Pts',(-1.14022195309742,-0.753299108715682,
5.24539077706077));
#6000=CARTESIAN_POINT('Ctrl Pts',(-1.11760842305144,-0.786458195591769,
5.2483024893283));
#6001=CARTESIAN_POINT('Ctrl Pts',(-1.05378026584285,-0.871729423492695,
5.25615182126945));
#6002=CARTESIAN_POINT('Ctrl Pts',(-1.01017024646971,-0.921910856948246,
5.26116046551499));
#6003=CARTESIAN_POINT('Ctrl Pts',(-0.914880073155494,-1.01664731801719,
5.27132508363935));
#6004=CARTESIAN_POINT('Ctrl Pts',(-0.8631561031155,-1.06091490904156,5.27646737636355));
#6005=CARTESIAN_POINT('Ctrl Pts',(-0.796430891736597,-1.10989744827673,
5.28250192610961));
#6006=CARTESIAN_POINT('Ctrl Pts',(-0.784373012541011,-1.11845139941638,
5.28357023595833));
#6007=CARTESIAN_POINT('Ctrl Pts',(-0.765644706481638,-1.13128551349674,
5.285193060773));
#6008=CARTESIAN_POINT('Ctrl Pts',(-0.759072336608693,-1.13570591499868,
5.2857558207428));
#6009=CARTESIAN_POINT('Ctrl Pts',(-0.746815869255001,-1.14379535674293,
5.28679231903699));
#6010=CARTESIAN_POINT('Ctrl Pts',(-0.741142663988383,-1.14747954877711,
5.28726695350393));
#6011=CARTESIAN_POINT('Ctrl Pts',(-0.727534349771829,-1.15617378617581,
5.28839362033158));
#6012=CARTESIAN_POINT('Ctrl Pts',(-0.719574614510532,-1.16114445297622,
5.28904318559633));
#6013=CARTESIAN_POINT('Ctrl Pts',(-0.691211850959365,-1.17845264563038,
5.2913269143071));
#6014=CARTESIAN_POINT('Ctrl Pts',(-0.67053653688783,-1.19033834549166,5.29293578638724));
#6015=CARTESIAN_POINT('Ctrl Pts',(-0.615354038592541,-1.2201668983377,5.29711361778615));
#6016=CARTESIAN_POINT('Ctrl Pts',(-0.580372681738932,-1.23718866756822,
5.29964649054921));
#6017=CARTESIAN_POINT('Ctrl Pts',(-0.452290400755728,-1.29288278544482,
5.30867415504866));
#6018=CARTESIAN_POINT('Ctrl Pts',(-0.355713277352951,-1.32271671026837,
5.31505421068723));
#6019=CARTESIAN_POINT('Ctrl Pts',(-0.230017874135355,-1.34676936383823,
5.32357250719713));
#6020=CARTESIAN_POINT('Ctrl Pts',(-0.203155593040073,-1.35108237578636,
5.32540302832876));
#6021=CARTESIAN_POINT('Ctrl Pts',(-0.161990942479023,-1.35643642718762,
5.32823381365224));
#6022=CARTESIAN_POINT('Ctrl Pts',(-0.147770369659149,-1.35805918061005,
5.32921632115055));
#6023=CARTESIAN_POINT('Ctrl Pts',(-0.121724195876615,-1.36061746241729,
5.33102561009702));
#6024=CARTESIAN_POINT('Ctrl Pts',(-0.109906763257582,-1.3616229826134,5.33185015462506));
#6025=CARTESIAN_POINT('Ctrl Pts',(-0.0839330299346769,-1.36349270808605,
5.33367117010073));
#6026=CARTESIAN_POINT('Ctrl Pts',(-0.069773499646246,-1.36429056669935,
5.33466958069469));
#6027=CARTESIAN_POINT('Ctrl Pts',(-0.0282458582375009,-1.36598239856109,
5.33761562348487));
#6028=CARTESIAN_POINT('Ctrl Pts',(-0.000861671889294049,-1.36627406128866,
5.33958115885716));
#6029=CARTESIAN_POINT('Ctrl Pts',(0.0631276116285825,-1.36503193223893,
5.34423021943495));
#6030=CARTESIAN_POINT('Ctrl Pts',(0.0996978597546384,-1.36284893754478,
5.34693045470113));
#6031=CARTESIAN_POINT('Ctrl Pts',(0.190805737046929,-1.35372382115644,5.35375654223748));
#6032=CARTESIAN_POINT('Ctrl Pts',(0.245095090711306,-1.34495458559843,5.35791508980577));
#6033=CARTESIAN_POINT('Ctrl Pts',(0.358292675106155,-1.31958753500389,5.36668807334671));
#6034=CARTESIAN_POINT('Ctrl Pts',(0.416922557012886,-1.30225258848866,5.37129244626548));
#6035=CARTESIAN_POINT('Ctrl Pts',(0.488221750774554,-1.27586013114751,5.37683696645621));
#6036=CARTESIAN_POINT('Ctrl Pts',(0.502158164396142,-1.27043959958545,5.37791782775316));
#6037=CARTESIAN_POINT('Ctrl Pts',(0.523369815070111,-1.26178577087957,5.37955559857019));
#6038=CARTESIAN_POINT('Ctrl Pts',(0.530710008758775,-1.25871608775739,5.38012097599131));
#6039=CARTESIAN_POINT('Ctrl Pts',(0.543609729075416,-1.25318849435541,5.38111164132233));
#6040=CARTESIAN_POINT('Ctrl Pts',(0.549180054904535,-1.25075745429931,5.38153840741199));
#6041=CARTESIAN_POINT('Ctrl Pts',(0.562844952468293,-1.24468483289101,5.38258303300933));
#6042=CARTESIAN_POINT('Ctrl Pts',(0.570920552161064,-1.24100141323936,5.38319843589929));
#6043=CARTESIAN_POINT('Ctrl Pts',(0.597543686662399,-1.22854325160766,5.38522266207002));
#6044=CARTESIAN_POINT('Ctrl Pts',(0.6159303474781,-1.21942892136342,5.38661320724766));
#6045=CARTESIAN_POINT('Ctrl Pts',(0.750144277404238,-1.14908789390465,5.3967590978939));
#6046=CARTESIAN_POINT('Ctrl Pts',(0.856839600941048,-1.07189221334997,5.40486173155934));
#6047=CARTESIAN_POINT('Ctrl Pts',(0.976508263362306,-0.955854902042567,
5.41584235714626));
#6048=CARTESIAN_POINT('Ctrl Pts',(1.00111929850485,-0.93004666468943,5.41822073983362));
#6049=CARTESIAN_POINT('Ctrl Pts',(1.03423753057966,-0.892478081839303,5.42162035765726));
#6050=CARTESIAN_POINT('Ctrl Pts',(1.04361113327111,-0.881498821501704,5.42260676229364));
#6051=CARTESIAN_POINT('Ctrl Pts',(1.06049228539495,-0.861079282695392,5.424429926698));
#6052=CARTESIAN_POINT('Ctrl Pts',(1.06805225483812,-0.851684086545846,5.42526450665598));
#6053=CARTESIAN_POINT('Ctrl Pts',(1.0832891177097,-0.832226438155453,5.42698506388635));
#6054=CARTESIAN_POINT('Ctrl Pts',(1.09095250973728,-0.822154948513786,5.42787145531561));
#6055=CARTESIAN_POINT('Ctrl Pts',(1.11014688234491,-0.796188096474105,5.43014709425882));
#6056=CARTESIAN_POINT('Ctrl Pts',(1.12147671116343,-0.78014838378125,5.43154372455901));
#6057=CARTESIAN_POINT('Ctrl Pts',(1.18274654006279,-0.689314419547003,5.439407566593));
#6058=CARTESIAN_POINT('Ctrl Pts',(1.22554263320739,-0.609986676872524,5.4461286100276));
#6059=CARTESIAN_POINT('Ctrl Pts',(1.29008659352131,-0.455654134637411,5.45877579098599));
#6060=CARTESIAN_POINT('Ctrl Pts',(1.31382524117489,-0.381849726491105,5.46465400960749));
#6061=CARTESIAN_POINT('Ctrl Pts',(1.33444165695525,-0.292287511987954,5.4713505685251));
#6062=CARTESIAN_POINT('Ctrl Pts',(1.33747116650936,-0.2780961104876,5.47239870322061));
#6063=CARTESIAN_POINT('Ctrl Pts',(1.34179286840774,-0.256143940649222,5.47399746886107));
#6064=CARTESIAN_POINT('Ctrl Pts',(1.34324502771044,-0.24841623008786,5.47455599157326));
#6065=CARTESIAN_POINT('Ctrl Pts',(1.3458245366006,-0.234004806969269,5.47558909379036));
#6066=CARTESIAN_POINT('Ctrl Pts',(1.34696893962538,-0.227324902049264,5.47606450673496));
#6067=CARTESIAN_POINT('Ctrl Pts',(1.34959571309199,-0.211275605672952,5.47719887739154));
#6068=CARTESIAN_POINT('Ctrl Pts',(1.35103028880671,-0.20189884111409,5.47785526807297));
#6069=CARTESIAN_POINT('Ctrl Pts',(1.35582855022567,-0.168191016632206,5.48019454771902));
#6070=CARTESIAN_POINT('Ctrl Pts',(1.35863375904979,-0.143783730602052,5.48185048809029));
#6071=CARTESIAN_POINT('Ctrl Pts',(1.36433716832411,-0.0787352919552279,
5.4861948317873));
#6072=CARTESIAN_POINT('Ctrl Pts',(1.36607844843105,-0.0380166348105744,
5.48884348979549));
#6073=CARTESIAN_POINT('Ctrl Pts',(1.36578123411808,0.11117059056373,5.49847555341945));
#6074=CARTESIAN_POINT('Ctrl Pts',(1.35265206358475,0.219197996974596,5.50534478210836));
#6075=CARTESIAN_POINT('Ctrl Pts',(1.32178242462068,0.345411612577719,5.51407081230514));
#6076=CARTESIAN_POINT('Ctrl Pts',(1.31618427225149,0.366165042277167,5.51552769550149));
#6077=CARTESIAN_POINT('Ctrl Pts',(1.30641000050486,0.399272670101188,5.51789234947613));
#6078=CARTESIAN_POINT('Ctrl Pts',(1.30254242451737,0.411714666666021,5.5187903138062));
#6079=CARTESIAN_POINT('Ctrl Pts',(1.29476509769958,0.435527121282318,5.52052790072583));
#6080=CARTESIAN_POINT('Ctrl Pts',(1.29088201792773,0.446905058302476,5.52136659431758));
#6081=CARTESIAN_POINT('Ctrl Pts',(1.28144141310626,0.473417154370428,5.52334147662694));
#6082=CARTESIAN_POINT('Ctrl Pts',(1.27576523518989,0.488506829522304,5.52448142605063));
#6083=CARTESIAN_POINT('Ctrl Pts',(1.25530444153453,0.540109634754774,5.52843674867076));
#6084=CARTESIAN_POINT('Ctrl Pts',(1.23920963753097,0.57607863434675,5.5312939596283));
#6085=CARTESIAN_POINT('Ctrl Pts',(1.19282653851386,0.668767933763115,5.53892664413396));
#6086=CARTESIAN_POINT('Ctrl Pts',(1.16005123739714,0.724130811923968,5.54376793987982));
#6087=CARTESIAN_POINT('Ctrl Pts',(1.0828975709452,0.835694697594957,5.55402808007369));
#6088=CARTESIAN_POINT('Ctrl Pts',(1.03774605386802,0.891143992435052,5.55943647808425));
#6089=CARTESIAN_POINT('Ctrl Pts',(0.978379082116922,0.953385461254074,5.56570511368386));
#6090=CARTESIAN_POINT('Ctrl Pts',(0.968125439883169,0.963795954522817,5.56676072056508));
#6091=CARTESIAN_POINT('Ctrl Pts',(0.952084494709027,0.979567900517138,5.56836840087211));
#6092=CARTESIAN_POINT('Ctrl Pts',(0.946414830089232,0.985046767434491,5.56892849619608));
#6093=CARTESIAN_POINT('Ctrl Pts',(0.935787226642523,0.995140257627,5.56996284312835));
#6094=CARTESIAN_POINT('Ctrl Pts',(0.930842154921886,0.999767348427093,5.57043795154724));
#6095=CARTESIAN_POINT('Ctrl Pts',(0.918916759775011,1.01076071869798,5.57156939394643));
#6096=CARTESIAN_POINT('Ctrl Pts',(0.91190447952565,1.01709167477767,5.57222319874144));
#6097=CARTESIAN_POINT('Ctrl Pts',(0.886632082052517,1.0394370623333,5.57454128184999));
#6098=CARTESIAN_POINT('Ctrl Pts',(0.868010180181264,1.05503760788256,5.57617925030358));
#6099=CARTESIAN_POINT('Ctrl Pts',(0.817629650011505,1.0950065196732,5.58045955421784));
#6100=CARTESIAN_POINT('Ctrl Pts',(0.785198449424994,1.11849065204015,5.58306357320232));
#6101=CARTESIAN_POINT('Ctrl Pts',(0.663750928290365,1.1985436753139,5.59245878758647));
#6102=CARTESIAN_POINT('Ctrl Pts',(0.569306889965283,1.24617829552289,5.59913517343118));
#6103=CARTESIAN_POINT('Ctrl Pts',(0.448303040506616,1.2905544036315,5.60776001354228));
#6104=CARTESIAN_POINT('Ctrl Pts',(0.42607595765485,1.29806219295615,5.6093453932261));
#6105=CARTESIAN_POINT('Ctrl Pts',(0.39072035355457,1.30899857776846,5.61187537921978));
#6106=CARTESIAN_POINT('Ctrl Pts',(0.37771460871665,1.31281046734407,5.61280774555333));
#6107=CARTESIAN_POINT('Ctrl Pts',(0.354331873442698,1.31928755790913,5.61448813871794));
#6108=CARTESIAN_POINT('Ctrl Pts',(0.343976047294522,1.32202541746576,5.61523378354662));
#6109=CARTESIAN_POINT('Ctrl Pts',(0.319519434279017,1.32818441806638,5.61699862891258));
#6110=CARTESIAN_POINT('Ctrl Pts',(0.305394463595379,1.3315031768989,5.61802096386402));
#6111=CARTESIAN_POINT('Ctrl Pts',(0.262713128041464,1.34081659251518,5.62112057963922));
#6112=CARTESIAN_POINT('Ctrl Pts',(0.234016556084462,1.34612159437641,5.62321874550225));
#6113=CARTESIAN_POINT('Ctrl Pts',(0.165533348248381,1.35652584155136,5.62826225691103));
#6114=CARTESIAN_POINT('Ctrl Pts',(0.125650014033341,1.36079948602555,5.63122867071618));
#6115=CARTESIAN_POINT('Ctrl Pts',(0.0345545374194687,1.36652184158529,5.63805614746475));
#6116=CARTESIAN_POINT('Ctrl Pts',(-0.0166685924520419,1.36685688322614,
5.64193316556925));
#6117=CARTESIAN_POINT('Ctrl Pts',(-0.126444224446211,1.36140257736312,5.65024299845795));
#6118=CARTESIAN_POINT('Ctrl Pts',(-0.184857527009722,1.35470810540855,5.65466560896516));
#6119=CARTESIAN_POINT('Ctrl Pts',(-0.257245702894402,1.34164087358332,5.66002866586836));
#6120=CARTESIAN_POINT('Ctrl Pts',(-0.271785382853547,1.33877120373766,5.66109966220259));
#6121=CARTESIAN_POINT('Ctrl Pts',(-0.294028003511482,1.33400389203126,5.66272568811305));
#6122=CARTESIAN_POINT('Ctrl Pts',(-0.301765437545236,1.33227492638884,5.66328901017658));
#6123=CARTESIAN_POINT('Ctrl Pts',(-0.315412074212977,1.32910053109462,5.66427793783087));
#6124=CARTESIAN_POINT('Ctrl Pts',(-0.321327069112466,1.32768291212253,5.66470499245999));
#6125=CARTESIAN_POINT('Ctrl Pts',(-0.335890166129764,1.32408961557647,5.66575274189337));
#6126=CARTESIAN_POINT('Ctrl Pts',(-0.344526749376954,1.32186869381107,5.66637094094005));
#6127=CARTESIAN_POINT('Ctrl Pts',(-0.373208878357486,1.31419278822845,5.66841532619139));
#6128=CARTESIAN_POINT('Ctrl Pts',(-0.393152697705361,1.30836486508455,5.66982273237149));
#6129=CARTESIAN_POINT('Ctrl Pts',(-0.524356055665068,1.26675360255849,5.67903488684609));
#6130=CARTESIAN_POINT('Ctrl Pts',(-0.630770161749997,1.21727104312232,5.68631932571444));
#6131=CARTESIAN_POINT('Ctrl Pts',(-0.768598042118655,1.13019543368379,5.69696101541999));
#6132=CARTESIAN_POINT('Ctrl Pts',(-0.806326397234676,1.10359492348215,5.70001382961969));
#6133=CARTESIAN_POINT('Ctrl Pts',(-0.856291253176667,1.0644352346191,5.70431022711215));
#6134=CARTESIAN_POINT('Ctrl Pts',(-0.869742486589888,1.05347284754225,5.70549377981104));
#6135=CARTESIAN_POINT('Ctrl Pts',(-0.892212626495895,1.03443657372131,5.70751972656323));
#6136=CARTESIAN_POINT('Ctrl Pts',(-0.901339892813703,1.02649343752124,5.70835686590052));
#6137=CARTESIAN_POINT('Ctrl Pts',(-0.919747968330122,1.01003872400555,5.71007534708974));
#6138=CARTESIAN_POINT('Ctrl Pts',(-0.929018977764569,1.00151798258327,5.710957016416));
#6139=CARTESIAN_POINT('Ctrl Pts',(-0.952209409305448,0.979605174984993,
5.71320477249114));
#6140=CARTESIAN_POINT('Ctrl Pts',(-0.965964612166757,0.966044180412237,
5.71457788387072));
#6141=CARTESIAN_POINT('Ctrl Pts',(-1.03714106876451,0.892832260762352,5.72190206385362));
#6142=CARTESIAN_POINT('Ctrl Pts',(-1.08932881502182,0.828353515204724,5.72806542448722));
#6143=CARTESIAN_POINT('Ctrl Pts',(-1.13941107388268,0.753492984586296,5.73486557418252));
#6144=CARTESIAN_POINT('Ctrl Pts',(-1.14342019818566,0.747395134825857,5.73541698282043));
#6145=CARTESIAN_POINT('Ctrl Pts',(-1.14737961474409,0.741266497064122,5.73596857206561));
#6146=CARTESIAN_POINT('Origin',(0.,0.,-1.10921167016993));
#6147=CARTESIAN_POINT('',(-1.14737960337948,0.741266514654979,6.45569480720057));
#6148=CARTESIAN_POINT('',(-1.14737960347042,0.741266514514221,6.33682691740051));
#6149=CARTESIAN_POINT('',(-1.14737960344596,0.741266514552077,-1.10921167016993));
#6150=CARTESIAN_POINT('Ctrl Pts',(-1.14737960337948,0.741266514654979,6.45569480720057));
#6151=CARTESIAN_POINT('Ctrl Pts',(-1.14440445020754,0.745871646546051,6.45530983005762));
#6152=CARTESIAN_POINT('Ctrl Pts',(-1.14140160089578,0.750458822460515,6.45492383550652));
#6153=CARTESIAN_POINT('Ctrl Pts',(-1.12652618635747,0.772886796456123,6.45302407185668));
#6154=CARTESIAN_POINT('Ctrl Pts',(-1.1142631691645,0.790463627220123,6.45149600304674));
#6155=CARTESIAN_POINT('Ctrl Pts',(-1.0331256952661,0.901118037528676,6.4416153273618));
#6156=CARTESIAN_POINT('Ctrl Pts',(-0.953074742876551,0.98539384339097,6.4328220089232));
#6157=CARTESIAN_POINT('Ctrl Pts',(-0.835074385669332,1.08163819922126,6.42132631641499));
#6158=CARTESIAN_POINT('Ctrl Pts',(-0.805849997455173,1.1035834900728,6.41858373599471));
#6159=CARTESIAN_POINT('Ctrl Pts',(-0.75695234810557,1.13732244969378,6.41419692716241));
#6160=CARTESIAN_POINT('Ctrl Pts',(-0.737800584619165,1.14983897029597,6.41252619215766));
#6161=CARTESIAN_POINT('Ctrl Pts',(-0.710516083765737,1.16670799891075,6.41022063931965));
#6162=CARTESIAN_POINT('Ctrl Pts',(-0.702641005517084,1.17146757936909,6.40956367510072));
#6163=CARTESIAN_POINT('Ctrl Pts',(-0.688983873355262,1.17953447453376,6.40843966839099));
#6164=CARTESIAN_POINT('Ctrl Pts',(-0.683224854159839,1.18287960491944,6.40797035453718));
#6165=CARTESIAN_POINT('Ctrl Pts',(-0.670531960670527,1.19012864759636,6.40694626238539));
#6166=CARTESIAN_POINT('Ctrl Pts',(-0.663588153550101,1.19401427067333,6.40639258875045));
#6167=CARTESIAN_POINT('Ctrl Pts',(-0.643512574817295,1.20501895154721,6.40480947527345));
#6168=CARTESIAN_POINT('Ctrl Pts',(-0.630297024991605,1.21198383370177,6.40378882476267));
#6169=CARTESIAN_POINT('Ctrl Pts',(-0.562731053724689,1.24618837029166,6.39866509343204));
#6170=CARTESIAN_POINT('Ctrl Pts',(-0.506714121456532,1.26999768900327,6.3947213613623));
#6171=CARTESIAN_POINT('Ctrl Pts',(-0.383234688998911,1.31300419079069,6.38629660361829));
#6172=CARTESIAN_POINT('Ctrl Pts',(-0.315510738722809,1.33090246850612,6.38183374219945));
#6173=CARTESIAN_POINT('Ctrl Pts',(-0.204589781098267,1.35127103821574,6.3744478966227));
#6174=CARTESIAN_POINT('Ctrl Pts',(-0.162127400519548,1.3570204703536,6.37160435668986));
#6175=CARTESIAN_POINT('Ctrl Pts',(-0.102927092378867,1.36221794305548,6.3675752874553));
#6176=CARTESIAN_POINT('Ctrl Pts',(-0.0863617076294256,1.36336837506538,
6.36644104216258));
#6177=CARTESIAN_POINT('Ctrl Pts',(-0.057670769968438,1.36483592444291,6.36446258564259));
#6178=CARTESIAN_POINT('Ctrl Pts',(-0.0455541280466855,1.36529404283025,
6.36362275807181));
#6179=CARTESIAN_POINT('Ctrl Pts',(-0.0205305648774539,1.36590668673522,
6.36187868208877));
#6180=CARTESIAN_POINT('Ctrl Pts',(-0.00762438340186637,1.36603968814276,
6.36097386201327));
#6181=CARTESIAN_POINT('Ctrl Pts',(0.0260383138641941,1.36590953713018,6.35859914428232));
#6182=CARTESIAN_POINT('Ctrl Pts',(0.0467896724752679,1.36535618087983,6.3571206211887));
#6183=CARTESIAN_POINT('Ctrl Pts',(0.172310182162419,1.35914429087719,6.34808380490484));
#6184=CARTESIAN_POINT('Ctrl Pts',(0.276137723201556,1.34190324070143,6.34017403794649));
#6185=CARTESIAN_POINT('Ctrl Pts',(0.418778274807004,1.3009514838768,6.3289602822008));
#6186=CARTESIAN_POINT('Ctrl Pts',(0.460013119199794,1.28694923642598,6.32568102972326));
#6187=CARTESIAN_POINT('Ctrl Pts',(0.524337441251927,1.26161879470272,6.32056312438273));
#6188=CARTESIAN_POINT('Ctrl Pts',(0.547897212024778,1.25156724842174,6.31868830675984));
#6189=CARTESIAN_POINT('Ctrl Pts',(0.57993169930762,1.2368219047728,6.31615113337325));
#6190=CARTESIAN_POINT('Ctrl Pts',(0.588658580463402,1.2326922930434,6.31546122077102));
#6191=CARTESIAN_POINT('Ctrl Pts',(0.603476008832462,1.2254873480536,6.31429286983384));
#6192=CARTESIAN_POINT('Ctrl Pts',(0.609588510114468,1.22245833886558,6.31381181996603));
#6193=CARTESIAN_POINT('Ctrl Pts',(0.622657850208297,1.21585950349539,6.31278550451638));
#6194=CARTESIAN_POINT('Ctrl Pts',(0.629607100958736,1.21227556137372,6.31224108079112));
#6195=CARTESIAN_POINT('Ctrl Pts',(0.649149352704366,1.20198364502491,6.31071265810335));
#6196=CARTESIAN_POINT('Ctrl Pts',(0.661668979811253,1.19513755111781,6.30973652712519));
#6197=CARTESIAN_POINT('Ctrl Pts',(0.742687226976892,1.14917094478586,6.30342448182142));
#6198=CARTESIAN_POINT('Ctrl Pts',(0.807803204980027,1.10437099698966,6.29836831671898));
#6199=CARTESIAN_POINT('Ctrl Pts',(0.937508247894822,0.997489452536332,6.28756297667497));
#6200=CARTESIAN_POINT('Ctrl Pts',(1.00059698491479,0.934189540578288,6.28182713684428));
#6201=CARTESIAN_POINT('Ctrl Pts',(1.06936175443099,0.850175472799675,6.27450893565179));
#6202=CARTESIAN_POINT('Ctrl Pts',(1.08133589564082,0.83489251682933,6.27318906818643));
#6203=CARTESIAN_POINT('Ctrl Pts',(1.10054750895023,0.809265319325732,6.27099075328883));
#6204=CARTESIAN_POINT('Ctrl Pts',(1.10797475919416,0.799066387210834,6.27011964889677));
#6205=CARTESIAN_POINT('Ctrl Pts',(1.12224387337831,0.77889087501064,6.2684028283803));
#6206=CARTESIAN_POINT('Ctrl Pts',(1.1290965978954,0.768923378854817,6.26755762471015));
#6207=CARTESIAN_POINT('Ctrl Pts',(1.14391003359632,0.746751711100486,6.2656833531759));
#6208=CARTESIAN_POINT('Ctrl Pts',(1.15180956849467,0.734508660117627,6.2646521693244));
#6209=CARTESIAN_POINT('Ctrl Pts',(1.17881781509049,0.691142712383491,6.26101139636744));
#6210=CARTESIAN_POINT('Ctrl Pts',(1.19687151723236,0.659384431595825,6.25836549542448));
#6211=CARTESIAN_POINT('Ctrl Pts',(1.27339882629084,0.511243761276505,6.24611053992899));
#6212=CARTESIAN_POINT('Ctrl Pts',(1.31630705305452,0.387612538287398,6.23603828958759));
#6213=CARTESIAN_POINT('Ctrl Pts',(1.34494681228947,0.23977049999888,6.22495936165501));
#6214=CARTESIAN_POINT('Ctrl Pts',(1.34837645728437,0.219665331900744,6.22347456644959));
#6215=CARTESIAN_POINT('Ctrl Pts',(1.35264792892096,0.190730128241583,6.22137554938291));
#6216=CARTESIAN_POINT('Ctrl Pts',(1.35385587282002,0.181957928923353,6.22074416382356));
#6217=CARTESIAN_POINT('Ctrl Pts',(1.35574842334905,0.167149928308582,6.21968738627107));
#6218=CARTESIAN_POINT('Ctrl Pts',(1.35647819818583,0.161120418052551,6.21925963351081));
#6219=CARTESIAN_POINT('Ctrl Pts',(1.35807178484605,0.14717482494711,6.21827625673913));
#6220=CARTESIAN_POINT('Ctrl Pts',(1.358906633699,0.139255774759589,6.21772219879438));
#6221=CARTESIAN_POINT('Ctrl Pts',(1.36111422127253,0.116400341995082,6.21613448632429));
#6222=CARTESIAN_POINT('Ctrl Pts',(1.36231031820514,0.101447552015138,6.21510972949913));
#6223=CARTESIAN_POINT('Ctrl Pts',(1.36716353701563,0.0249396662897132,6.20992388297698));
#6224=CARTESIAN_POINT('Ctrl Pts',(1.3668963603584,-0.0367988979956117,6.20592696799781));
#6225=CARTESIAN_POINT('Ctrl Pts',(1.35737839888966,-0.168700863544685,6.19740924188006));
#6226=CARTESIAN_POINT('Ctrl Pts',(1.34685286961724,-0.238585335064236,6.19290607094659));
#6227=CARTESIAN_POINT('Ctrl Pts',(1.32164607377661,-0.347745789026422,6.18556117799279));
#6228=CARTESIAN_POINT('Ctrl Pts',(1.31048223161538,-0.387700007231746,6.18280552681886));
#6229=CARTESIAN_POINT('Ctrl Pts',(1.2923943968099,-0.442652727132081,6.17888197866998));
#6230=CARTESIAN_POINT('Ctrl Pts',(1.28698958831601,-0.458129320828903,6.17776192967536));
#6231=CARTESIAN_POINT('Ctrl Pts',(1.27712896707764,-0.48481226516603,6.17580252845228));
#6232=CARTESIAN_POINT('Ctrl Pts',(1.27280076988883,-0.496064023090694,6.17496739486579));
#6233=CARTESIAN_POINT('Ctrl Pts',(1.26353118474063,-0.519241321798936,6.17322784884794));
#6234=CARTESIAN_POINT('Ctrl Pts',(1.25856855822918,-0.531157009807242,6.1723228040802));
#6235=CARTESIAN_POINT('Ctrl Pts',(1.24512112689277,-0.562198471790177,6.16993588974925));
#6236=CARTESIAN_POINT('Ctrl Pts',(1.23636474060115,-0.581202103264453,6.16844513204998));
#6237=CARTESIAN_POINT('Ctrl Pts',(1.18135137566068,-0.693721256429585,6.1594351305149));
#6238=CARTESIAN_POINT('Ctrl Pts',(1.12494786305416,-0.78187273542734,6.15156768497056));
#6239=CARTESIAN_POINT('Ctrl Pts',(1.03111454543118,-0.897061554814988,6.14033238585897));
#6240=CARTESIAN_POINT('Ctrl Pts',(1.00149475503274,-0.930013607369452,6.13699264760518));
#6241=CARTESIAN_POINT('Ctrl Pts',(0.952112153077906,-0.979851019272929,
6.13179510033943));
#6242=CARTESIAN_POINT('Ctrl Pts',(0.933379017009408,-0.997712076012414,
6.12989955628111));
#6243=CARTESIAN_POINT('Ctrl Pts',(0.906970681146503,-1.02149571236173,6.12734193330027));
#6244=CARTESIAN_POINT('Ctrl Pts',(0.899724343702005,-1.02788395550298,6.12665146230513));
#6245=CARTESIAN_POINT('Ctrl Pts',(0.887263110893025,-1.03863679787903,6.12548409710729));
#6246=CARTESIAN_POINT('Ctrl Pts',(0.882082403951631,-1.04304020383841,6.12500455656652));
#6247=CARTESIAN_POINT('Ctrl Pts',(0.870910816259394,-1.05239285686619,6.12398303847046));
#6248=CARTESIAN_POINT('Ctrl Pts',(0.864910288107302,-1.05732992773473,6.12344187774078));
#6249=CARTESIAN_POINT('Ctrl Pts',(0.847928940834887,-1.07106040846325,6.12193033182987));
#6250=CARTESIAN_POINT('Ctrl Pts',(0.836853601307326,-1.07973606761225,6.12096756579873));
#6251=CARTESIAN_POINT('Ctrl Pts',(0.760817502329282,-1.13742454254391,6.11449728121188));
#6252=CARTESIAN_POINT('Ctrl Pts',(0.691715274520605,-1.18072488413482,6.10929006046853));
#6253=CARTESIAN_POINT('Ctrl Pts',(0.567250484647958,-1.24401542546841,6.10031400487418));
#6254=CARTESIAN_POINT('Ctrl Pts',(0.51370719297801,-1.26706425570585,6.0965679762011));
#6255=CARTESIAN_POINT('Ctrl Pts',(0.423821986447855,-1.29912073507177,6.09028582856094));
#6256=CARTESIAN_POINT('Ctrl Pts',(0.388291503652538,-1.31017903012344,6.0878048761877));
#6257=CARTESIAN_POINT('Ctrl Pts',(0.337074086496683,-1.32385318457558,6.0842044664804));
#6258=CARTESIAN_POINT('Ctrl Pts',(0.3217226887629,-1.32766737954676,6.0831223836814));
#6259=CARTESIAN_POINT('Ctrl Pts',(0.294626135083744,-1.33390222928798,6.08120542220118));
#6260=CARTESIAN_POINT('Ctrl Pts',(0.282908681953205,-1.33643644762305,6.08037419378321));
#6261=CARTESIAN_POINT('Ctrl Pts',(0.258242016487869,-1.34143235863214,6.07861884304774));
#6262=CARTESIAN_POINT('Ctrl Pts',(0.245287551443216,-1.34386149116407,6.07769379805122));
#6263=CARTESIAN_POINT('Ctrl Pts',(0.210414047757166,-1.34987970005337,6.07519411535882));
#6264=CARTESIAN_POINT('Ctrl Pts',(0.188440085098363,-1.35312213359127,6.07360902260546));
#6265=CARTESIAN_POINT('Ctrl Pts',(0.0753841768797939,-1.3669972563527,6.06539775923293));
#6266=CARTESIAN_POINT('Ctrl Pts',(-0.0165087501760205,-1.36897278954647,
6.05851537358678));
#6267=CARTESIAN_POINT('Ctrl Pts',(-0.158953219622941,-1.35768687377814,
6.04770758090593));
#6268=CARTESIAN_POINT('Ctrl Pts',(-0.209750261559177,-1.35077202641308,
6.04383083264569));
#6269=CARTESIAN_POINT('Ctrl Pts',(-0.287761429526375,-1.33564467113485,
6.0379297681569));
#6270=CARTESIAN_POINT('Ctrl Pts',(-0.315311021690413,-1.32941059993486,
6.0358566520489));
#6271=CARTESIAN_POINT('Ctrl Pts',(-0.352298666655904,-1.31982612694721,
6.03310439248042));
#6272=CARTESIAN_POINT('Ctrl Pts',(-0.361920435123491,-1.31722016746267,
6.03239133086418));
#6273=CARTESIAN_POINT('Ctrl Pts',(-0.378107732938875,-1.31264523167021,
6.03119756511241));
#6274=CARTESIAN_POINT('Ctrl Pts',(-0.384688406119156,-1.31073178064364,
6.03071392181081));
#6275=CARTESIAN_POINT('Ctrl Pts',(-0.398572135039674,-1.30658125738923,
6.02969736262084));
#6276=CARTESIAN_POINT('Ctrl Pts',(-0.405871245646881,-1.30433234572426,
6.02916510129971));
#6277=CARTESIAN_POINT('Ctrl Pts',(-0.426324834242277,-1.29784211309081,
6.02767871498929));
#6278=CARTESIAN_POINT('Ctrl Pts',(-0.439434773335473,-1.29346207193785,
6.02673197952802));
#6279=CARTESIAN_POINT('Ctrl Pts',(-0.534104287670281,-1.26022730997512,
6.01992359983421));
#6280=CARTESIAN_POINT('Ctrl Pts',(-0.612836336047709,-1.22387739829746,
6.01440581546567));
#6281=CARTESIAN_POINT('Ctrl Pts',(-0.759231301078887,-1.13859327465452,
6.00351144808931));
#6282=CARTESIAN_POINT('Ctrl Pts',(-0.826899319098853,-1.09044121198202,
5.99815820758992));
#6283=CARTESIAN_POINT('Ctrl Pts',(-0.904440483505733,-1.02387334794342,
5.9912686712639));
#6284=CARTESIAN_POINT('Ctrl Pts',(-0.918829536599898,-1.01098043591348,
5.98995512418428));
#6285=CARTESIAN_POINT('Ctrl Pts',(-0.942139537993689,-0.989185381330332,
5.987764686366));
#6286=CARTESIAN_POINT('Ctrl Pts',(-0.951219622387305,-0.980456954393349,
5.98689503877151));
#6287=CARTESIAN_POINT('Ctrl Pts',(-0.968785917618262,-0.96309725571591,
5.98517916100943));
#6288=CARTESIAN_POINT('Ctrl Pts',(-0.977280678003605,-0.954476263679363,
5.98433341916004));
#6289=CARTESIAN_POINT('Ctrl Pts',(-0.99767685882617,-0.933219248255586,
5.98226260526604));
#6290=CARTESIAN_POINT('Ctrl Pts',(-1.00945386027575,-0.920467345826625,
5.98103246779922));
#6291=CARTESIAN_POINT('Ctrl Pts',(-1.05159886445962,-0.873051785552421,
5.97649973291954));
#6292=CARTESIAN_POINT('Ctrl Pts',(-1.08044761741099,-0.8370852399255,5.97313842627058));
#6293=CARTESIAN_POINT('Ctrl Pts',(-1.17589104567685,-0.704921059882282,
5.96105327948384));
#6294=CARTESIAN_POINT('Ctrl Pts',(-1.23189474927965,-0.601718948704819,
5.95203582672786));
#6295=CARTESIAN_POINT('Ctrl Pts',(-1.28156798426731,-0.473256692169054,
5.94189766057578));
#6296=CARTESIAN_POINT('Ctrl Pts',(-1.28862410383586,-0.453691996609041,
5.94038288996042));
#6297=CARTESIAN_POINT('Ctrl Pts',(-1.29806536655051,-0.425513677613729,
5.93824975337007));
#6298=CARTESIAN_POINT('Ctrl Pts',(-1.30081672326878,-0.417026916630356,
5.93761349974809));
#6299=CARTESIAN_POINT('Ctrl Pts',(-1.30530417774433,-0.402708348064585,
5.93655112927669));
#6300=CARTESIAN_POINT('Ctrl Pts',(-1.30708474808069,-0.396891013779978,
5.9361225930048));
#6301=CARTESIAN_POINT('Ctrl Pts',(-1.31109587051744,-0.383466369127569,
5.9351408493504));
#6302=CARTESIAN_POINT('Ctrl Pts',(-1.31329915579811,-0.375851264781785,
5.93458916630575));
#6303=CARTESIAN_POINT('Ctrl Pts',(-1.31942870003773,-0.353953796880181,
5.93301653595154));
#6304=CARTESIAN_POINT('Ctrl Pts',(-1.32318925783754,-0.339625701442354,
5.93200421434232));
#6305=CARTESIAN_POINT('Ctrl Pts',(-1.34065302965984,-0.268387318971649,
5.92704036557674));
#6306=CARTESIAN_POINT('Ctrl Pts',(-1.35092281608484,-0.21069252994807,5.92323653002666));
#6307=CARTESIAN_POINT('Ctrl Pts',(-1.36310831423466,-0.102232810880837,
5.91619935983331));
#6308=CARTESIAN_POINT('Ctrl Pts',(-1.36595936467849,-0.0516798434778776,
5.91296421690439));
#6309=CARTESIAN_POINT('Ctrl Pts',(-1.366047001476,0.0586057802240502,5.90582635074415));
#6310=CARTESIAN_POINT('Ctrl Pts',(-1.362181923725,0.118229610721552,5.90191469227535));
#6311=CARTESIAN_POINT('Ctrl Pts',(-1.35201016131709,0.19588768243336,5.89662787991302));
#6312=CARTESIAN_POINT('Ctrl Pts',(-1.34921135206583,0.214317829707607,5.89535915937795));
#6313=CARTESIAN_POINT('Ctrl Pts',(-1.34412573925723,0.24373718572544,5.89330841556674));
#6314=CARTESIAN_POINT('Ctrl Pts',(-1.34207903734226,0.25476589893796,5.8925338501391));
#6315=CARTESIAN_POINT('Ctrl Pts',(-1.33753296025065,0.277685426158528,5.89091142799491));
#6316=CARTESIAN_POINT('Ctrl Pts',(-1.33501029714375,0.289570553369898,5.89006290951559));
#6317=CARTESIAN_POINT('Ctrl Pts',(-1.32859364054022,0.317933294837616,5.8880199565238));
#6318=CARTESIAN_POINT('Ctrl Pts',(-1.32455125394838,0.334374896836102,5.8868209794133));
#6319=CARTESIAN_POINT('Ctrl Pts',(-1.30844645651988,0.394994840010479,5.88234354358863));
#6320=CARTESIAN_POINT('Ctrl Pts',(-1.29447161457298,0.438629073356744,5.87900658410948));
#6321=CARTESIAN_POINT('Ctrl Pts',(-1.24785192896617,0.562405982736412,5.86920991196423));
#6322=CARTESIAN_POINT('Ctrl Pts',(-1.2097545625888,0.640255153364024,5.86261965587765));
#6323=CARTESIAN_POINT('Ctrl Pts',(-1.15894021175953,0.723138427875389,5.85530498938922));
#6324=CARTESIAN_POINT('Ctrl Pts',(-1.15321303393221,0.73223715878447,5.85449793769901));
#6325=CARTESIAN_POINT('Ctrl Pts',(-1.14737959943097,0.741266520766746,5.85369350940778));
#6326=CARTESIAN_POINT('',(-1.36599948656567,0.000864816812998655,5.78997189030577));
#6327=CARTESIAN_POINT('Ctrl Pts',(-1.14737961474409,0.741266497064122,5.73596857206561));
#6328=CARTESIAN_POINT('Ctrl Pts',(-1.1904390391621,0.674616370563709,5.74196721228499));
#6329=CARTESIAN_POINT('Ctrl Pts',(-1.22761917360703,0.604325674625206,5.74799784971009));
#6330=CARTESIAN_POINT('Ctrl Pts',(-1.26385745663935,0.518469722964953,5.75477595797064));
#6331=CARTESIAN_POINT('Ctrl Pts',(-1.26903215898028,0.50567177192747,5.75577147868141));
#6332=CARTESIAN_POINT('Ctrl Pts',(-1.27676541420663,0.485679235051532,5.75730143114503));
#6333=CARTESIAN_POINT('Ctrl Pts',(-1.27945899464218,0.478538327087086,5.75784296259488));
#6334=CARTESIAN_POINT('Ctrl Pts',(-1.28445557466837,0.464948131192376,5.75886375145181));
#6335=CARTESIAN_POINT('Ctrl Pts',(-1.28677004381773,0.458503810711634,5.75934358414366));
#6336=CARTESIAN_POINT('Ctrl Pts',(-1.29233212524565,0.442643063548985,5.76051474460296));
#6337=CARTESIAN_POINT('Ctrl Pts',(-1.29552538832794,0.433208017806375,5.76120303571006));
#6338=CARTESIAN_POINT('Ctrl Pts',(-1.30736921686815,0.396910689697875,5.76382194096085));
#6339=CARTESIAN_POINT('Ctrl Pts',(-1.31529041836771,0.369815814102299,5.76571640831512));
#6340=CARTESIAN_POINT('Ctrl Pts',(-1.35126590273527,0.230914257858472,5.77521477579502));
#6341=CARTESIAN_POINT('Ctrl Pts',(-1.36592675483423,0.116128576340583,5.78240718741147));
#6342=CARTESIAN_POINT('Ctrl Pts',(-1.36599972625862,0.000864789789742776,
5.78997147629599));
#6343=CARTESIAN_POINT('Ctrl Pts',(-1.14737960347042,0.741266514514221,6.33682691740051));
#6344=CARTESIAN_POINT('Ctrl Pts',(-1.14723096453265,0.741496587345168,6.33680902383529));
#6345=CARTESIAN_POINT('Ctrl Pts',(-1.14708225500945,0.741726617610742,6.33679112826742));
#6346=CARTESIAN_POINT('Ctrl Pts',(-1.12525165515805,0.77547285771292,6.33416500414653));
#6347=CARTESIAN_POINT('Ctrl Pts',(-1.10211318795007,0.808019388345351,6.33151930391138));
#6348=CARTESIAN_POINT('Ctrl Pts',(-1.07059991158523,0.848469820141379,6.32801762349369));
#6349=CARTESIAN_POINT('Ctrl Pts',(-1.06350279087134,0.857348819772749,6.32723504209464));
#6350=CARTESIAN_POINT('Ctrl Pts',(-1.05223168284591,0.871094468075964,6.32599963840549));
#6351=CARTESIAN_POINT('Ctrl Pts',(-1.04813264084159,0.876022288293213,6.32555183897138));
#6352=CARTESIAN_POINT('Ctrl Pts',(-1.03948157824367,0.88627485665296,6.32460939732392));
#6353=CARTESIAN_POINT('Ctrl Pts',(-1.03492304926233,0.891593712006638,6.32411425894315));
#6354=CARTESIAN_POINT('Ctrl Pts',(-1.02321928075941,0.905038891851274,6.32284720487594));
#6355=CARTESIAN_POINT('Ctrl Pts',(-1.01601812235669,0.9131156818452,6.32207150324614));
#6356=CARTESIAN_POINT('Ctrl Pts',(-0.984084033010925,0.948087367889869,
6.31865159366154));
#6357=CARTESIAN_POINT('Ctrl Pts',(-0.958375517571697,0.974067203004257,
6.31595015759383));
#6358=CARTESIAN_POINT('Ctrl Pts',(-0.869195900675413,1.05723681358068,6.30682937812303));
#6359=CARTESIAN_POINT('Ctrl Pts',(-0.801405968763932,1.10950471419032,6.30030422555004));
#6360=CARTESIAN_POINT('Ctrl Pts',(-0.682668169963466,1.18445981664098,6.28982482379678));
#6361=CARTESIAN_POINT('Ctrl Pts',(-0.634425256535374,1.21098590210553,6.28578812494159));
#6362=CARTESIAN_POINT('Ctrl Pts',(-0.568053821610563,1.24242120255726,6.28052933440924));
#6363=CARTESIAN_POINT('Ctrl Pts',(-0.551240836551429,1.24997167475445,6.27922092291943));
#6364=CARTESIAN_POINT('Ctrl Pts',(-0.523987835425009,1.26155372288526,6.2771367374175));
#6365=CARTESIAN_POINT('Ctrl Pts',(-0.513642627249782,1.26580105545935,6.27635390555899));
#6366=CARTESIAN_POINT('Ctrl Pts',(-0.491919902409015,1.27440936873442,6.27472693046606));
#6367=CARTESIAN_POINT('Ctrl Pts',(-0.480533807818921,1.2787461459087,6.27388364134074));
#6368=CARTESIAN_POINT('Ctrl Pts',(-0.45301878601578,1.28880674524566,6.27186756907271));
#6369=CARTESIAN_POINT('Ctrl Pts',(-0.436837103257292,1.29438102427092,6.27069969966985));
#6370=CARTESIAN_POINT('Ctrl Pts',(-0.375459820246054,1.31424212702984,6.26633131726732));
#6371=CARTESIAN_POINT('Ctrl Pts',(-0.329633485626932,1.32647838928624,6.26319520891731));
#6372=CARTESIAN_POINT('Ctrl Pts',(-0.191334400224435,1.35579390127283,6.25397054412427));
#6373=CARTESIAN_POINT('Ctrl Pts',(-0.0976491674684298,1.36574129866363,
6.24804701724237));
#6374=CARTESIAN_POINT('Ctrl Pts',(0.033993280002979,1.36609677200363,6.23942680174019));
#6375=CARTESIAN_POINT('Ctrl Pts',(0.0716597263597227,1.36463924751874,6.23692372875893));
#6376=CARTESIAN_POINT('Ctrl Pts',(0.120374236612702,1.36073193415394,6.23358444143237));
#6377=CARTESIAN_POINT('Ctrl Pts',(0.131522648630233,1.35969964545806,6.23281325655067));
#6378=CARTESIAN_POINT('Ctrl Pts',(0.149006497069655,1.35786370043844,6.23159107075647));
#6379=CARTESIAN_POINT('Ctrl Pts',(0.155351423310136,1.35715242185572,6.23114489233996));
#6380=CARTESIAN_POINT('Ctrl Pts',(0.168684834346834,1.35556299594173,6.23020127260897));
#6381=CARTESIAN_POINT('Ctrl Pts',(0.175671872813295,1.35467523587653,6.22970328607124));
#6382=CARTESIAN_POINT('Ctrl Pts',(0.193559226041958,1.35226179829853,6.22841991884293));
#6383=CARTESIAN_POINT('Ctrl Pts',(0.20444835674903,1.35065835603961,6.22763056677145));
#6384=CARTESIAN_POINT('Ctrl Pts',(0.253589639516747,1.34281437758426,6.22403513984802));
#6385=CARTESIAN_POINT('Ctrl Pts',(0.291581993739851,1.33507959679299,6.22116467483921));
#6386=CARTESIAN_POINT('Ctrl Pts',(0.425778015598182,1.30175783987426,6.2108068676161));
#6387=CARTESIAN_POINT('Ctrl Pts',(0.519467878813218,1.26728718328051,6.20319381413474));
#6388=CARTESIAN_POINT('Ctrl Pts',(0.646023166964252,1.20430858652762,6.19275250421038));
#6389=CARTESIAN_POINT('Ctrl Pts',(0.682593097560144,1.18396469732931,6.18971022100872));
#6390=CARTESIAN_POINT('Ctrl Pts',(0.732521085941029,1.15310592738439,6.18552090943373));
#6391=CARTESIAN_POINT('Ctrl Pts',(0.746702037525502,1.14397400907077,6.18432662354723));
#6392=CARTESIAN_POINT('Ctrl Pts',(0.770691846055378,1.12788939300134,6.1822976436892));
#6393=CARTESIAN_POINT('Ctrl Pts',(0.780584403000371,1.12106574761171,6.18145837105975));
#6394=CARTESIAN_POINT('Ctrl Pts',(0.800767046223592,1.10674755226151,6.17974006956903));
#6395=CARTESIAN_POINT('Ctrl Pts',(0.81104502831989,1.09923791219301,6.1788617122077));
#6396=CARTESIAN_POINT('Ctrl Pts',(0.837201690498609,1.07955984577203,6.17661652434054));
#6397=CARTESIAN_POINT('Ctrl Pts',(0.852921088848621,1.06718405886742,6.1752577173778));
#6398=CARTESIAN_POINT('Ctrl Pts',(0.933020639030918,1.00122130650264,6.1682712458327));
#6399=CARTESIAN_POINT('Ctrl Pts',(0.992646369926603,0.9421396147417,6.16286934869321));
#6400=CARTESIAN_POINT('Ctrl Pts',(1.10038364310237,0.813721818013225,6.15209304523007));
#6401=CARTESIAN_POINT('Ctrl Pts',(1.14824159036326,0.744664307084841,6.14673745338958));
#6402=CARTESIAN_POINT('Ctrl Pts',(1.19630848763014,0.659542186703067,6.14010820120531));
#6403=CARTESIAN_POINT('Ctrl Pts',(1.20296912258001,0.647313792807427,6.13915503519501));
#6404=CARTESIAN_POINT('Ctrl Pts',(1.21303789253717,0.628136077809906,6.13765553426122));
#6405=CARTESIAN_POINT('Ctrl Pts',(1.21657606252696,0.621255613780105,6.13711663523172));
#6406=CARTESIAN_POINT('Ctrl Pts',(1.22311842145835,0.608262862044143,6.13609658311447));
#6407=CARTESIAN_POINT('Ctrl Pts',(1.22613563931947,0.602157593822545,6.1356162079459));
#6408=CARTESIAN_POINT('Ctrl Pts',(1.23335085452847,0.587278697820586,6.13444324049325));
#6409=CARTESIAN_POINT('Ctrl Pts',(1.23750097292051,0.578482434696092,6.13374793939764));
#6410=CARTESIAN_POINT('Ctrl Pts',(1.25254815887428,0.545686568089057,6.13115070926833));
#6411=CARTESIAN_POINT('Ctrl Pts',(1.26284316913252,0.521418869291389,6.12921932471899));
#6412=CARTESIAN_POINT('Ctrl Pts',(1.28902359909137,0.454373766959362,6.12388468202372));
#6413=CARTESIAN_POINT('Ctrl Pts',(1.30347793977487,0.411074434611565,6.12044163577528));
#6414=CARTESIAN_POINT('Ctrl Pts',(1.34304350979749,0.269279620973568,6.10930789038274));
#6415=CARTESIAN_POINT('Ctrl Pts',(1.3593515329279,0.168664785083447,6.1016514097853));
#6416=CARTESIAN_POINT('Ctrl Pts',(1.36539363505839,0.0459182219369729,6.09280556149921));
#6417=CARTESIAN_POINT('Ctrl Pts',(1.36594307473127,0.0246549835607194,6.09128944628695));
#6418=CARTESIAN_POINT('Ctrl Pts',(1.36602798545492,-0.00959514265164508,
6.08887207555029));
#6419=CARTESIAN_POINT('Ctrl Pts',(1.36587511343861,-0.0225769547362636,
6.08796152522914));
#6420=CARTESIAN_POINT('Ctrl Pts',(1.36522392435435,-0.0475867251530467,
6.08621764183283));
#6421=CARTESIAN_POINT('Ctrl Pts',(1.36475163931352,-0.0596140849356033,
6.08538359696397));
#6422=CARTESIAN_POINT('Ctrl Pts',(1.36326944676234,-0.0878393676983431,
6.08343622962519));
#6423=CARTESIAN_POINT('Ctrl Pts',(1.36212971955882,-0.104028859829275,6.08232696011955));
#6424=CARTESIAN_POINT('Ctrl Pts',(1.35716597624842,-0.160222425983841,6.07849947578572));
#6425=CARTESIAN_POINT('Ctrl Pts',(1.35186551179989,-0.200077020791389,6.07582581843807));
#6426=CARTESIAN_POINT('Ctrl Pts',(1.33313060226053,-0.30521252492663,6.06881603736694));
#6427=CARTESIAN_POINT('Ctrl Pts',(1.3166663428574,-0.369840757963558,6.06455525745848));
#6428=CARTESIAN_POINT('Ctrl Pts',(1.2741352518087,-0.497091773021355,6.05592326830799));
#6429=CARTESIAN_POINT('Ctrl Pts',(1.24799574870182,-0.559486689925425,6.05156198322036));
#6430=CARTESIAN_POINT('Ctrl Pts',(1.21061009477214,-0.632929778636938,6.04598541681214));
#6431=CARTESIAN_POINT('Ctrl Pts',(1.20365216067483,-0.646063725657715,6.04496978901454));
#6432=CARTESIAN_POINT('Ctrl Pts',(1.19265225892561,-0.66603271850596,6.04339316741588));
#6433=CARTESIAN_POINT('Ctrl Pts',(1.18876243903611,-0.672950851425942,6.04284086889513));
#6434=CARTESIAN_POINT('Ctrl Pts',(1.1817862463817,-0.685108930773588,6.04185873120822));
#6435=CARTESIAN_POINT('Ctrl Pts',(1.17872481232108,-0.690362796339865,6.04143042701915));
#6436=CARTESIAN_POINT('Ctrl Pts',(1.17109456295627,-0.70325869912298,6.04036960701642));
#6437=CARTESIAN_POINT('Ctrl Pts',(1.16648603138621,-0.710876642511075,6.03973468844069));
#6438=CARTESIAN_POINT('Ctrl Pts',(1.15092238847172,-0.736044611485236,6.03761078878561));
#6439=CARTESIAN_POINT('Ctrl Pts',(1.13964360669512,-0.753389906973071,6.03610412269872));
#6440=CARTESIAN_POINT('Ctrl Pts',(1.06225131740906,-0.866692843627718,6.02600589851431));
#6441=CARTESIAN_POINT('Ctrl Pts',(0.984484890517809,-0.954110476343341,
6.01702115446776));
#6442=CARTESIAN_POINT('Ctrl Pts',(0.861468540129706,-1.0611273908183,6.00493010243138));
#6443=CARTESIAN_POINT('Ctrl Pts',(0.824837296202431,-1.08984571466828,6.00153588986857));
#6444=CARTESIAN_POINT('Ctrl Pts',(0.772591504234391,-1.1266591443182,5.99696893006937));
#6445=CARTESIAN_POINT('Ctrl Pts',(0.758184301068697,-1.13640445044443,5.99573621283639));
#6446=CARTESIAN_POINT('Ctrl Pts',(0.73343877328153,-1.15246263817196,5.9936625166208));
#6447=CARTESIAN_POINT('Ctrl Pts',(0.723195794720574,-1.15891778209984,5.99281643566034));
#6448=CARTESIAN_POINT('Ctrl Pts',(0.702135726468353,-1.17180190925377,5.99110105987824));
#6449=CARTESIAN_POINT('Ctrl Pts',(0.691312902544989,-1.17821932673476,5.99023223913466));
#6450=CARTESIAN_POINT('Ctrl Pts',(0.663699862792933,-1.19408104011411,5.98804632150419));
#6451=CARTESIAN_POINT('Ctrl Pts',(0.646795362803002,-1.20332159379481,5.98673640757605));
#6452=CARTESIAN_POINT('Ctrl Pts',(0.558138420305705,-1.24937605664431,5.98000058958578));
#6453=CARTESIAN_POINT('Ctrl Pts',(0.483421757123601,-1.28014242796536,5.97478416574482));
#6454=CARTESIAN_POINT('Ctrl Pts',(0.320980846549595,-1.33076517826726,5.96384058841696));
#6455=CARTESIAN_POINT('Ctrl Pts',(0.233144320857145,-1.34892698356517,5.95814464289484));
#6456=CARTESIAN_POINT('Ctrl Pts',(0.130774740134236,-1.35979249242472,5.95115331696106));
#6457=CARTESIAN_POINT('Ctrl Pts',(0.117352384735143,-1.36101654605131,5.95022954192214));
#6458=CARTESIAN_POINT('Ctrl Pts',(0.0963719359629294,-1.36261721525101,
5.94877145333579));
#6459=CARTESIAN_POINT('Ctrl Pts',(0.0888246926803422,-1.36312999832691,
5.94824408864919));
#6460=CARTESIAN_POINT('Ctrl Pts',(0.0744100192719718,-1.3639891597929,5.94723075704724));
#6461=CARTESIAN_POINT('Ctrl Pts',(0.0675436133213621,-1.36434641151483,
5.94674536234453));
#6462=CARTESIAN_POINT('Ctrl Pts',(0.0505577907766123,-1.36510163403285,
5.9455383247655));
#6463=CARTESIAN_POINT('Ctrl Pts',(0.0404362169862525,-1.36543892506649,
5.94481358244947));
#6464=CARTESIAN_POINT('Ctrl Pts',(0.000681321907970434,-1.36632132337396,
5.9419477857565));
#6465=CARTESIAN_POINT('Ctrl Pts',(-0.0289607774440487,-1.36601442383707,
5.93976924873405));
#6466=CARTESIAN_POINT('Ctrl Pts',(-0.114282003861064,-1.36235293538809,
5.93341836936025));
#6467=CARTESIAN_POINT('Ctrl Pts',(-0.169796274916512,-1.35655248938338,
5.92918954302956));
#6468=CARTESIAN_POINT('Ctrl Pts',(-0.308709648445458,-1.3333759661935,5.91854150290063));
#6469=CARTESIAN_POINT('Ctrl Pts',(-0.391141898439683,-1.31156601464212,
5.91217251747732));
#6470=CARTESIAN_POINT('Ctrl Pts',(-0.49206495959233,-1.27449235482162,5.90441887640844));
#6471=CARTESIAN_POINT('Ctrl Pts',(-0.512918083284765,-1.26624398588903,
5.90281812290129));
#6472=CARTESIAN_POINT('Ctrl Pts',(-0.545725724285701,-1.2523234765058,5.90030034868819));
#6473=CARTESIAN_POINT('Ctrl Pts',(-0.557816427376738,-1.2469849682473,5.89937258813855));
#6474=CARTESIAN_POINT('Ctrl Pts',(-0.58070321766845,-1.23648006713151,5.89761594750999));
#6475=CARTESIAN_POINT('Ctrl Pts',(-0.591512530231947,-1.23134565652511,
5.89678609450838));
#6476=CARTESIAN_POINT('Ctrl Pts',(-0.616350975457051,-1.21914485348429,
5.89487789614863));
#6477=CARTESIAN_POINT('Ctrl Pts',(-0.630328644966801,-1.21197711707044,
5.89380310398349));
#6478=CARTESIAN_POINT('Ctrl Pts',(-0.676364210674887,-1.18735820471018,
5.89025659022246));
#6479=CARTESIAN_POINT('Ctrl Pts',(-0.707847527346664,-1.16886281874683,
5.88782068480353));
#6480=CARTESIAN_POINT('Ctrl Pts',(-0.786044769648155,-1.11860474209448,
5.88169728982519));
#6481=CARTESIAN_POINT('Ctrl Pts',(-0.831599416638986,-1.08516631497758,
5.87806114292099));
#6482=CARTESIAN_POINT('Ctrl Pts',(-0.939825610390796,-0.994896710889066,
5.86900051111617));
#6483=CARTESIAN_POINT('Ctrl Pts',(-0.999528290433561,-0.934896299024387,
5.86360740352212));
#6484=CARTESIAN_POINT('Ctrl Pts',(-1.06213219289128,-0.859082987100705,
5.85693898454604));
#6485=CARTESIAN_POINT('Ctrl Pts',(-1.07079979400966,-0.848254760128754,
5.85598946138802));
#6486=CARTESIAN_POINT('Ctrl Pts',(-1.08403605887532,-0.831192822520132,
5.85449443661436));
#6487=CARTESIAN_POINT('Ctrl Pts',(-1.08871950066444,-0.825048802582859,
5.85395629900024));
#6488=CARTESIAN_POINT('Ctrl Pts',(-1.09743583884147,-0.81341073603355,5.85293666768306));
#6489=CARTESIAN_POINT('Ctrl Pts',(-1.10148012134357,-0.807925726583716,
5.85245593781119));
#6490=CARTESIAN_POINT('Ctrl Pts',(-1.11121229182865,-0.794517695498988,
5.85128066071818));
#6491=CARTESIAN_POINT('Ctrl Pts',(-1.11685660277803,-0.786563691411526,
5.85058337908918));
#6492=CARTESIAN_POINT('Ctrl Pts',(-1.13755359943611,-0.756725384917957,
5.84796933254502));
#6493=CARTESIAN_POINT('Ctrl Pts',(-1.15205123712983,-0.734465267145847,
5.84602264320846));
#6494=CARTESIAN_POINT('Ctrl Pts',(-1.20296072227006,-0.651078132416014,
5.83877983945842));
#6495=CARTESIAN_POINT('Ctrl Pts',(-1.23523019366588,-0.587556792199495,
5.83336380620333));
#6496=CARTESIAN_POINT('Ctrl Pts',(-1.2904223139448,-0.454032510265899,5.82246364282492));
#6497=CARTESIAN_POINT('Ctrl Pts',(-1.31293869255956,-0.38409650211287,5.81700142079563));
#6498=CARTESIAN_POINT('Ctrl Pts',(-1.33489839526453,-0.29070904672298,5.81008138536126));
#6499=CARTESIAN_POINT('Ctrl Pts',(-1.33951995424586,-0.268611010201654,
5.80846955967288));
#6500=CARTESIAN_POINT('Ctrl Pts',(-1.34598137816927,-0.233378634483755,
5.80593868475107));
#6501=CARTESIAN_POINT('Ctrl Pts',(-1.34818121501188,-0.220315434738023,
5.80500870020211));
#6502=CARTESIAN_POINT('Ctrl Pts',(-1.35194437230554,-0.195795919405125,
5.80327812258695));
#6503=CARTESIAN_POINT('Ctrl Pts',(-1.35355292069266,-0.184347858791772,
5.80247620477624));
#6504=CARTESIAN_POINT('Ctrl Pts',(-1.35648370817036,-0.161376701461312,
5.8008786273071));
#6505=CARTESIAN_POINT('Ctrl Pts',(-1.35780490106219,-0.149854445707179,
5.8000830625301));
#6506=CARTESIAN_POINT('Ctrl Pts',(-1.36095380321471,-0.118916025686271,
5.79796127990866));
#6507=CARTESIAN_POINT('Ctrl Pts',(-1.36251278902884,-0.0994748039951829,
5.7966431664332));
#6508=CARTESIAN_POINT('Ctrl Pts',(-1.36523487203515,-0.0530785383892744,
5.79352797295233));
#6509=CARTESIAN_POINT('Ctrl Pts',(-1.36601683429475,-0.0261093149545231,
5.79174167536384));
#6510=CARTESIAN_POINT('Ctrl Pts',(-1.36599972525692,0.00086637060349483,
5.78997137255369));
#6511=CARTESIAN_POINT('Origin',(0.,0.,3.44061240069463));
#6512=CARTESIAN_POINT('',(-1.70824949798349,0.00130963321928915,0.193190200199919));
#6513=CARTESIAN_POINT('',(0.747616516620363,1.53872147257634,4.34771760247897E-5));
#6514=CARTESIAN_POINT('Ctrl Pts',(-1.70971129366951,0.00131075390815409,
0.193190200199919));
#6515=CARTESIAN_POINT('Ctrl Pts',(-1.7103415218327,0.0801238654015101,0.188773164585797));
#6516=CARTESIAN_POINT('Ctrl Pts',(-1.66983493919842,0.719618324757823,0.152894693722701));
#6517=CARTESIAN_POINT('Ctrl Pts',(-0.899480193612338,1.76907630764895,0.0885124527147331));
#6518=CARTESIAN_POINT('Ctrl Pts',(0.28909851215658,1.75784256997736,0.0285472473208922));
#6519=CARTESIAN_POINT('Ctrl Pts',(0.747616516620363,1.53872147257634,4.34771760247897E-5));
#6520=CARTESIAN_POINT('',(-0.746545333137425,1.53648564199954,0.));
#6521=CARTESIAN_POINT('Origin',(0.,0.,0.));
#6522=CARTESIAN_POINT('',(-1.70829001772743,0.00184159784217005,0.106809799800075));
#6523=CARTESIAN_POINT('Ctrl Pts',(-0.746545333137426,1.53648564199954,6.93889390390723E-16));
#6524=CARTESIAN_POINT('Ctrl Pts',(-1.25276108530162,1.2905262935952,0.0314614352489755));
#6525=CARTESIAN_POINT('Ctrl Pts',(-1.67270494886694,0.709596610538724,0.0670647018490002));
#6526=CARTESIAN_POINT('Ctrl Pts',(-1.71019420630271,0.0756867134818199,
0.102667968449025));
#6527=CARTESIAN_POINT('Ctrl Pts',(-1.70960986444288,0.00184302068421545,
0.106809799800075));
#6528=CARTESIAN_POINT('',(-1.70824999635299,0.000111624363083944,0.70680979975714));
#6529=CARTESIAN_POINT('Ctrl Pts',(-1.70824900736989,0.00184155363153534,
0.106809799800075));
#6530=CARTESIAN_POINT('Ctrl Pts',(-1.70831458995836,-0.0589937051053382,
0.110224750287315));
#6531=CARTESIAN_POINT('Ctrl Pts',(-1.70512614389993,-0.119972079441817,
0.113639700774556));
#6532=CARTESIAN_POINT('Ctrl Pts',(-1.69866513901472,-0.180706413821171,
0.117054651261796));
#6533=CARTESIAN_POINT('Ctrl Pts',(-1.69225479648065,-0.240964515133158,
0.120442824270333));
#6534=CARTESIAN_POINT('Ctrl Pts',(-1.68262305022738,-0.300981850843056,
0.123830997278869));
#6535=CARTESIAN_POINT('Ctrl Pts',(-1.66980391133269,-0.360378911977436,
0.127219170287406));
#6536=CARTESIAN_POINT('Ctrl Pts',(-1.65699495703225,-0.419728783127227,
0.130604651448416));
#6537=CARTESIAN_POINT('Ctrl Pts',(-1.64100373423955,-0.478458836454786,
0.133990132609428));
#6538=CARTESIAN_POINT('Ctrl Pts',(-1.621915776411,-0.536197050280131,0.137375613770439));
#6539=CARTESIAN_POINT('Ctrl Pts',(-1.60283531726547,-0.593912581712318,
0.140759764948937));
#6540=CARTESIAN_POINT('Ctrl Pts',(-1.58066070057341,-0.650636540481587,
0.144143916127434));
#6541=CARTESIAN_POINT('Ctrl Pts',(-1.55552739778889,-0.706011740148935,
0.147528067305932));
#6542=CARTESIAN_POINT('Ctrl Pts',(-1.53000373790585,-0.762246997981248,
0.150964779321592));
#6543=CARTESIAN_POINT('Ctrl Pts',(-1.50142888312398,-0.81709070658417,0.154401491337252));
#6544=CARTESIAN_POINT('Ctrl Pts',(-1.46999459697372,-0.870191902610033,
0.157838203352912));
#6545=CARTESIAN_POINT('Ctrl Pts',(-1.43900897726615,-0.922535177027307,
0.161225862644827));
#6546=CARTESIAN_POINT('Ctrl Pts',(-1.40524538544557,-0.973184946985413,
0.164613521936742));
#6547=CARTESIAN_POINT('Ctrl Pts',(-1.36893126062472,-1.02183426551687,0.168001181228657));
#6548=CARTESIAN_POINT('Ctrl Pts',(-1.33182840238382,-1.07154023469262,0.171462419606189));
#6549=CARTESIAN_POINT('Ctrl Pts',(-1.29206326804371,-1.11915736418746,0.174923657983722));
#6550=CARTESIAN_POINT('Ctrl Pts',(-1.24991976686571,-1.16439625510321,0.178384896361254));
#6551=CARTESIAN_POINT('Ctrl Pts',(-1.2077762656877,-1.20963514601895,0.181846134738786));
#6552=CARTESIAN_POINT('Ctrl Pts',(-1.1632548734801,-1.25249545114912,0.185307373116318));
#6553=CARTESIAN_POINT('Ctrl Pts',(-1.11667462808752,-1.29273192792845,0.18876861149385));
#6554=CARTESIAN_POINT('Ctrl Pts',(-1.06980461621609,-1.33321870785881,0.192251381549643));
#6555=CARTESIAN_POINT('Ctrl Pts',(-1.02063842807767,-1.37123223284083,0.195734151605436));
#6556=CARTESIAN_POINT('Ctrl Pts',(-0.969466967790923,-1.40650341658393,
0.199216921661229));
#6557=CARTESIAN_POINT('Ctrl Pts',(-0.918081535653809,-1.44192208567155,
0.202714254810377));
#6558=CARTESIAN_POINT('Ctrl Pts',(-0.864674369909386,-1.47457504324174,
0.206211587959525));
#6559=CARTESIAN_POINT('Ctrl Pts',(-0.809575461633486,-1.50422924929046,
0.209708921108673));
#6560=CARTESIAN_POINT('Ctrl Pts',(-0.754852679879619,-1.53368102422513,
0.213182380105048));
#6561=CARTESIAN_POINT('Ctrl Pts',(-0.698461622166891,-1.56017460403329,
0.216655839101424));
#6562=CARTESIAN_POINT('Ctrl Pts',(-0.640754405190757,-1.58352513549,0.220129298097799));
#6563=CARTESIAN_POINT('Ctrl Pts',(-0.583081702786774,-1.60686170104011,
0.22360067962523));
#6564=CARTESIAN_POINT('Ctrl Pts',(-0.524094870000844,-1.6270587575761,0.227072061152661));
#6565=CARTESIAN_POINT('Ctrl Pts',(-0.464167575172626,-1.64397886989413,
0.230543442680092));
#6566=CARTESIAN_POINT('Ctrl Pts',(-0.404254501418413,-1.66089496697719,
0.234014000429747));
#6567=CARTESIAN_POINT('Ctrl Pts',(-0.343401894943893,-1.67453552683196,
0.237484558179402));
#6568=CARTESIAN_POINT('Ctrl Pts',(-0.281998295476573,-1.6848130530858,0.240955115929057));
#6569=CARTESIAN_POINT('Ctrl Pts',(-0.219782145675592,-1.69522658125907,
0.244471599371701));
#6570=CARTESIAN_POINT('Ctrl Pts',(-0.157000829752451,-1.70218728839646,
0.247988082814344));
#6571=CARTESIAN_POINT('Ctrl Pts',(-0.0940666075405792,-1.70565809465022,
0.251504566256987));
#6572=CARTESIAN_POINT('Ctrl Pts',(-0.0318790834905831,-1.70908772069138,
0.254979327539086));
#6573=CARTESIAN_POINT('Ctrl Pts',(0.0304572233450804,-1.7091098811712,0.258454088821184));
#6574=CARTESIAN_POINT('Ctrl Pts',(0.0925444116386326,-1.70574136209874,
0.261928850103282));
#6575=CARTESIAN_POINT('Ctrl Pts',(0.155749840047458,-1.70231217329296,0.265466194626198));
#6576=CARTESIAN_POINT('Ctrl Pts',(0.218696542192045,-1.69536899906895,0.269003539149113));
#6577=CARTESIAN_POINT('Ctrl Pts',(0.280972685895826,-1.6849843952632,0.272540883672029));
#6578=CARTESIAN_POINT('Ctrl Pts',(0.343248829599607,-1.67459979145744,0.276078228194944));
#6579=CARTESIAN_POINT('Ctrl Pts',(0.404853895881334,-1.6607739382837,0.27961557271786));
#6580=CARTESIAN_POINT('Ctrl Pts',(0.465392026083252,-1.64363266107672,0.283152917240776));
#6581=CARTESIAN_POINT('Ctrl Pts',(0.524997251490571,-1.62675553440822,0.286635750571249));
#6582=CARTESIAN_POINT('Ctrl Pts',(0.583797434628291,-1.6065996069445,0.290118583901722));
#6583=CARTESIAN_POINT('Ctrl Pts',(0.641407914169682,-1.58326054398526,0.293601417232194));
#6584=CARTESIAN_POINT('Ctrl Pts',(0.699258108267395,-1.55982436825822,0.297098742472007));
#6585=CARTESIAN_POINT('Ctrl Pts',(0.755908164860664,-1.53317858765772,0.30059606771182));
#6586=CARTESIAN_POINT('Ctrl Pts',(0.810982201756074,-1.50347129368501,0.304093392951633));
#6587=CARTESIAN_POINT('Ctrl Pts',(0.865685923739254,-1.47396374998629,0.307567202361443));
#6588=CARTESIAN_POINT('Ctrl Pts',(0.918834298152729,-1.44143596599254,0.311041011771252));
#6589=CARTESIAN_POINT('Ctrl Pts',(0.970079538891547,-1.4060809901012,0.314514821181061));
#6590=CARTESIAN_POINT('Ctrl Pts',(1.02129571686976,-1.37074606510992,0.317986660486139));
#6591=CARTESIAN_POINT('Ctrl Pts',(1.07061048676336,-1.33258741489734,0.321458499791217));
#6592=CARTESIAN_POINT('Ctrl Pts',(1.11770390797386,-1.29184210977966,0.324930339096295));
#6593=CARTESIAN_POINT('Ctrl Pts',(1.16478760702395,-1.25110521629108,0.328401461660524));
#6594=CARTESIAN_POINT('Ctrl Pts',(1.20965048620019,-1.20778305899605,0.331872584224754));
#6595=CARTESIAN_POINT('Ctrl Pts',(1.25200621942742,-1.16215252398946,0.335343706788983));
#6596=CARTESIAN_POINT('Ctrl Pts',(1.29491110305326,-1.11593038013611,0.338859833138876));
#6597=CARTESIAN_POINT('Ctrl Pts',(1.33524297221629,-1.06733993260901,0.34237595948877));
#6598=CARTESIAN_POINT('Ctrl Pts',(1.37274487765719,-1.01670524901072,0.345892085838663));
#6599=CARTESIAN_POINT('Ctrl Pts',(1.40981438688767,-0.966654382289095,0.349367671322935));
#6600=CARTESIAN_POINT('Ctrl Pts',(1.44411862471989,-0.914606640349092,0.352843256807207));
#6601=CARTESIAN_POINT('Ctrl Pts',(1.47545332507607,-0.860903913350356,0.356318842291478));
#6602=CARTESIAN_POINT('Ctrl Pts',(1.50733627948133,-0.806261565509918,0.359855239074182));
#6603=CARTESIAN_POINT('Ctrl Pts',(1.5361445182402,-0.749906239244957,0.363391635856886));
#6604=CARTESIAN_POINT('Ctrl Pts',(1.56171302119027,-0.692221425516987,0.36692803263959));
#6605=CARTESIAN_POINT('Ctrl Pts',(1.58728152414033,-0.634536611789017,0.370464429422294));
#6606=CARTESIAN_POINT('Ctrl Pts',(1.60961015864768,-0.575522842169992,0.374000826204998));
#6607=CARTESIAN_POINT('Ctrl Pts',(1.6285871045859,-0.515579387947677,0.377537222987702));
#6608=CARTESIAN_POINT('Ctrl Pts',(1.64722044712831,-0.45672129142701,0.381009588500704));
#6609=CARTESIAN_POINT('Ctrl Pts',(1.6626970729652,-0.39673127692693,0.384481954013706));
#6610=CARTESIAN_POINT('Ctrl Pts',(1.6748836768792,-0.335980254514478,0.387954319526707));
#6611=CARTESIAN_POINT('Ctrl Pts',(1.68716247160561,-0.274769654835853,0.391452953243704));
#6612=CARTESIAN_POINT('Ctrl Pts',(1.69610102240621,-0.212786956690893,0.394951586960701));
#6613=CARTESIAN_POINT('Ctrl Pts',(1.70161369856505,-0.150428997722399,0.398450220677697));
#6614=CARTESIAN_POINT('Ctrl Pts',(1.70707003818485,-0.088708303031531,0.401913100269235));
#6615=CARTESIAN_POINT('Ctrl Pts',(1.70917014433344,-0.026620498361166,0.405375979860772));
#6616=CARTESIAN_POINT('Ctrl Pts',(1.70788233348107,0.0354400547864655,0.408838859452309));
#6617=CARTESIAN_POINT('Ctrl Pts',(1.70659530809443,0.0974627557620102,0.412299626953194));
#6618=CARTESIAN_POINT('Ctrl Pts',(1.70192447367992,0.15945773039416,0.415760394454078));
#6619=CARTESIAN_POINT('Ctrl Pts',(1.6938902172817,0.221029396907651,0.419221161954963));
#6620=CARTESIAN_POINT('Ctrl Pts',(1.68585791093812,0.282586118900111,0.422681089467008));
#6621=CARTESIAN_POINT('Ctrl Pts',(1.67446386916949,0.343719232323013,0.426141016979053));
#6622=CARTESIAN_POINT('Ctrl Pts',(1.6597802429042,0.404039116627186,0.429600944491098));
#6623=CARTESIAN_POINT('Ctrl Pts',(1.64481317494788,0.465523370665447,0.433127659844726));
#6624=CARTESIAN_POINT('Ctrl Pts',(1.62642826834427,0.52616212671388,0.436654375198354));
#6625=CARTESIAN_POINT('Ctrl Pts',(1.60475580541016,0.58555688664927,0.440181090551981));
#6626=CARTESIAN_POINT('Ctrl Pts',(1.58346741409825,0.643899073932092,0.443645306719844));
#6627=CARTESIAN_POINT('Ctrl Pts',(1.55900731654214,0.701040549287598,0.447109522887707));
#6628=CARTESIAN_POINT('Ctrl Pts',(1.53154746996109,0.756624351812561,0.45057373905557));
#6629=CARTESIAN_POINT('Ctrl Pts',(1.50334450373795,0.813712365780093,0.45413170400208));
#6630=CARTESIAN_POINT('Ctrl Pts',(1.47197732711775,0.869156660332305,0.457689668948589));
#6631=CARTESIAN_POINT('Ctrl Pts',(1.43768090094917,0.922600503764211,0.461247633895098));
#6632=CARTESIAN_POINT('Ctrl Pts',(1.4033844747806,0.976044347196117,0.464805598841607));
#6633=CARTESIAN_POINT('Ctrl Pts',(1.36615919110336,1.02748731456081,0.468363563788117));
#6634=CARTESIAN_POINT('Ctrl Pts',(1.32628400933715,1.07660985926964,0.471921528734626));
#6635=CARTESIAN_POINT('Ctrl Pts',(1.2873024587237,1.12463153285235,0.475399757158923));
#6636=CARTESIAN_POINT('Ctrl Pts',(1.24563210246975,1.17062859785337,0.47887798558322));
#6637=CARTESIAN_POINT('Ctrl Pts',(1.20151108135262,1.21428546227271,0.482356214007517));
#6638=CARTESIAN_POINT('Ctrl Pts',(1.15714051720953,1.25818924450528,0.485854114860602));
#6639=CARTESIAN_POINT('Ctrl Pts',(1.1102917499648,1.2997258249965,0.489352015713686));
#6640=CARTESIAN_POINT('Ctrl Pts',(1.06124904461688,1.3386069355116,0.492849916566771));
#6641=CARTESIAN_POINT('Ctrl Pts',(1.01261269947674,1.3771658832089,0.496318834358923));
#6642=CARTESIAN_POINT('Ctrl Pts',(0.961819031833934,1.41311287122005,0.499787752151075));
#6643=CARTESIAN_POINT('Ctrl Pts',(0.909181379826556,1.44620443958545,0.503256669943226));
#6644=CARTESIAN_POINT('Ctrl Pts',(0.856575039118757,1.47927632356201,0.506723524263318));
#6645=CARTESIAN_POINT('Ctrl Pts',(0.802127317729894,1.50949588715465,0.510190378583409));
#6646=CARTESIAN_POINT('Ctrl Pts',(0.746181120237089,1.53666255186418,0.513657232903501));
#6647=CARTESIAN_POINT('Ctrl Pts',(0.690247857302824,1.56382293573907,0.517123285699412));
#6648=CARTESIAN_POINT('Ctrl Pts',(0.632817262007056,1.58793160091938,0.520589338495322));
#6649=CARTESIAN_POINT('Ctrl Pts',(0.57425565462772,1.6088345177886,0.524055391291232));
#6650=CARTESIAN_POINT('Ctrl Pts',(0.514767864255296,1.63006802541475,0.527576261557092));
#6651=CARTESIAN_POINT('Ctrl Pts',(0.454113466530574,1.64799327853745,0.531097131822953));
#6652=CARTESIAN_POINT('Ctrl Pts',(0.392693999809817,1.66250097293607,0.534618002088813));
#6653=CARTESIAN_POINT('Ctrl Pts',(0.332155549922089,1.67680056518636,0.538088368074243));
#6654=CARTESIAN_POINT('Ctrl Pts',(0.270874358340689,1.68777998316324,0.541558734059672));
#6655=CARTESIAN_POINT('Ctrl Pts',(0.209244251076581,1.69538635888443,0.545029100045102));
#6656=CARTESIAN_POINT('Ctrl Pts',(0.146268788207356,1.70315877812988,0.548575222451177));
#6657=CARTESIAN_POINT('Ctrl Pts',(0.0829295507635524,1.70740908443476,0.552121344857253));
#6658=CARTESIAN_POINT('Ctrl Pts',(0.0196484347567886,1.70813699729021,0.555667467263328));
#6659=CARTESIAN_POINT('Ctrl Pts',(-0.0436326812499752,1.70886491014566,
0.559213589669403));
#6660=CARTESIAN_POINT('Ctrl Pts',(-0.106855121658145,1.70607051955128,0.562759712075477));
#6661=CARTESIAN_POINT('Ctrl Pts',(-0.169603612446375,1.69980960026267,0.566305834481553));
#6662=CARTESIAN_POINT('Ctrl Pts',(-0.231141829633215,1.69366943966069,0.56978356036874));
#6663=CARTESIAN_POINT('Ctrl Pts',(-0.292468277930089,1.68417100072598,0.573261286255928));
#6664=CARTESIAN_POINT('Ctrl Pts',(-0.353188497672923,1.67133956681805,0.576739012143115));
#6665=CARTESIAN_POINT('Ctrl Pts',(-0.414262064020097,1.65843346348995,0.580236975813338));
#6666=CARTESIAN_POINT('Ctrl Pts',(-0.474721801697741,1.64215542820075,0.583734939483562));
#6667=CARTESIAN_POINT('Ctrl Pts',(-0.534170512454316,1.62258433559686,0.587232903153786));
#6668=CARTESIAN_POINT('Ctrl Pts',(-0.59311744304232,1.60317843389485,0.590701342065982));
#6669=CARTESIAN_POINT('Ctrl Pts',(-0.651069855630353,1.580535001617,0.594169780978179));
#6670=CARTESIAN_POINT('Ctrl Pts',(-0.707652173206536,1.55478180599596,0.597638219890375));
#6671=CARTESIAN_POINT('Ctrl Pts',(-0.76420099665976,1.52904385507923,0.601104605646668));
#6672=CARTESIAN_POINT('Ctrl Pts',(-0.819380872878149,1.50020000119686,0.60457099140296));
#6673=CARTESIAN_POINT('Ctrl Pts',(-0.872835779942873,1.46842628815733,0.608037377159252));
#6674=CARTESIAN_POINT('Ctrl Pts',(-0.926278498929028,1.43665981973822,0.611502972556263));
#6675=CARTESIAN_POINT('Ctrl Pts',(-0.977996594013848,1.40196507765051,0.614968567953273));
#6676=CARTESIAN_POINT('Ctrl Pts',(-1.02766004585383,1.36456326077456,0.618434163350284));
#6677=CARTESIAN_POINT('Ctrl Pts',(-1.07812221834835,1.32655992301053,0.6219554947568));
#6678=CARTESIAN_POINT('Ctrl Pts',(-1.1264626182537,1.28576195469007,0.625476826163317));
#6679=CARTESIAN_POINT('Ctrl Pts',(-1.17236898279256,1.24244477973306,0.628998157569833));
#6680=CARTESIAN_POINT('Ctrl Pts',(-1.21760539790529,1.1997597680239,0.632468099283903));
#6681=CARTESIAN_POINT('Ctrl Pts',(-1.26047804564556,1.15462901610646,0.635938040997972));
#6682=CARTESIAN_POINT('Ctrl Pts',(-1.3007262878688,1.10735233171157,0.639407982712041));
#6683=CARTESIAN_POINT('Ctrl Pts',(-1.34186864228173,1.05902539872268,0.642955008964781));
#6684=CARTESIAN_POINT('Ctrl Pts',(-1.38026822661701,1.00845647137167,0.64650203521752));
#6685=CARTESIAN_POINT('Ctrl Pts',(-1.4156926497375,0.955998108773865,0.65004906147026));
#6686=CARTESIAN_POINT('Ctrl Pts',(-1.451117072858,0.903539746176061,0.653596087722999));
#6687=CARTESIAN_POINT('Ctrl Pts',(-1.48356610494929,0.849192461909207,0.657143113975739));
#6688=CARTESIAN_POINT('Ctrl Pts',(-1.51285789915611,0.793334128511411,0.660690140228478));
#6689=CARTESIAN_POINT('Ctrl Pts',(-1.54459640063931,0.73281001773563,0.6645334451892));
#6690=CARTESIAN_POINT('Ctrl Pts',(-1.5727487797283,0.670282551675062,0.668376750149923));
#6691=CARTESIAN_POINT('Ctrl Pts',(-1.59707520162033,0.606192100632624,0.672220055110644));
#6692=CARTESIAN_POINT('Ctrl Pts',(-1.62023120184969,0.545185245385863,0.675878446424705));
#6693=CARTESIAN_POINT('Ctrl Pts',(-1.63992068276636,0.482762784725111,0.679536837738766));
#6694=CARTESIAN_POINT('Ctrl Pts',(-1.65598315357621,0.419330248815646,0.683195229052827));
#6695=CARTESIAN_POINT('Ctrl Pts',(-1.67201517077544,0.356017977700565,0.686846684246917));
#6696=CARTESIAN_POINT('Ctrl Pts',(-1.68443374424877,0.291699846434291,0.690498139441006));
#6697=CARTESIAN_POINT('Ctrl Pts',(-1.69312744441239,0.226798411541141,0.694149594635095));
#6698=CARTESIAN_POINT('Ctrl Pts',(-1.70180113708534,0.162046339385127,0.697792646450381));
#6699=CARTESIAN_POINT('Ctrl Pts',(-1.70676696174966,0.0967140536837641,
0.701435698265668));
#6700=CARTESIAN_POINT('Ctrl Pts',(-1.70796442270991,0.0312344882654268,
0.705078750080954));
#6701=CARTESIAN_POINT('Ctrl Pts',(-1.70815408644173,0.0208632952600976,
0.705655766639683));
#6702=CARTESIAN_POINT('Ctrl Pts',(-1.7082493182883,0.0104884272114703,0.706232783198412));
#6703=CARTESIAN_POINT('Ctrl Pts',(-1.70824999635299,0.000111624363083394,
0.70680979975714));
#6704=CARTESIAN_POINT('',(-1.70824952897253,-0.00126856813606742,1.30680979980007));
#6705=CARTESIAN_POINT('Ctrl Pts',(-1.70824999635304,0.000111623590999127,
0.706809799800073));
#6706=CARTESIAN_POINT('Ctrl Pts',(-1.70825423774439,-0.0647972069556505,
0.710419145624602));
#6707=CARTESIAN_POINT('Ctrl Pts',(-1.70455463276262,-0.129644182097538,
0.714028491449132));
#6708=CARTESIAN_POINT('Ctrl Pts',(-1.69719806951645,-0.194001998261928,
0.717637837273661));
#6709=CARTESIAN_POINT('Ctrl Pts',(-1.68982284212325,-0.258523094983278,
0.721256340276473));
#6710=CARTESIAN_POINT('Ctrl Pts',(-1.67877217615949,-0.3225521131443,0.724874843279286));
#6711=CARTESIAN_POINT('Ctrl Pts',(-1.66414446627173,-0.385669881993904,
0.728493346282097));
#6712=CARTESIAN_POINT('Ctrl Pts',(-1.64949678221494,-0.448873838291371,
0.73211679035847));
#6713=CARTESIAN_POINT('Ctrl Pts',(-1.63126244491383,-0.511163641249322,
0.735740234434843));
#6714=CARTESIAN_POINT('Ctrl Pts',(-1.60958946394413,-0.572136190133131,
0.739363678511216));
#6715=CARTESIAN_POINT('Ctrl Pts',(-1.5878610510406,-0.63326468555238,0.742996390095023));
#6716=CARTESIAN_POINT('Ctrl Pts',(-1.56267659384783,-0.693068787128632,
0.746629101678831));
#6717=CARTESIAN_POINT('Ctrl Pts',(-1.53423184058334,-0.751166241147904,
0.750261813262638));
#6718=CARTESIAN_POINT('Ctrl Pts',(-1.52167059471973,-0.776822164305316,
0.751866024166894));
#6719=CARTESIAN_POINT('Ctrl Pts',(-1.50847414164659,-0.802145619181886,
0.753470235071149));
#6720=CARTESIAN_POINT('Ctrl Pts',(-1.49466204101235,-0.827105462233683,
0.755074445975405));
#6721=CARTESIAN_POINT('Ctrl Pts',(-1.4647228023275,-0.881208651781241,0.758551748554876));
#6722=CARTESIAN_POINT('Ctrl Pts',(-1.43178256343332,-0.933791892404183,
0.762029051134347));
#6723=CARTESIAN_POINT('Ctrl Pts',(-1.39602016698291,-0.98450279627688,0.765506353713818));
#6724=CARTESIAN_POINT('Ctrl Pts',(-1.36004473689107,-1.03551578081488,0.769004370297506));
#6725=CARTESIAN_POINT('Ctrl Pts',(-1.32121360177983,-1.08463355996619,0.772502386881194));
#6726=CARTESIAN_POINT('Ctrl Pts',(-1.27975602779576,-1.13152223655588,0.776000403464882));
#6727=CARTESIAN_POINT('Ctrl Pts',(-1.23865440931033,-1.17800832609929,0.779468386013347));
#6728=CARTESIAN_POINT('Ctrl Pts',(-1.19497160965764,-1.22230304805398,0.782936368561813));
#6729=CARTESIAN_POINT('Ctrl Pts',(-1.14897319366195,-1.26411180785018,0.786404351110279));
#6730=CARTESIAN_POINT('Ctrl Pts',(-1.10300215759204,-1.30589568155596,0.789870269389731));
#6731=CARTESIAN_POINT('Ctrl Pts',(-1.05471861327783,-1.34519618714438,0.793336187669184));
#6732=CARTESIAN_POINT('Ctrl Pts',(-1.0044247665779,-1.38175574932219,0.796802105948637));
#6733=CARTESIAN_POINT('Ctrl Pts',(-0.954142538812777,-1.41830686547335,
0.800267223528179));
#6734=CARTESIAN_POINT('Ctrl Pts',(-0.901851340961412,-1.45211799742215,
0.803732341107722));
#6735=CARTESIAN_POINT('Ctrl Pts',(-0.84788460589561,-1.48297328282921,0.807197458687265));
#6736=CARTESIAN_POINT('Ctrl Pts',(-0.79303548095234,-1.51433307145434,0.810719233106853));
#6737=CARTESIAN_POINT('Ctrl Pts',(-0.736455979813227,-1.54263917879348,
0.814241007526442));
#6738=CARTESIAN_POINT('Ctrl Pts',(-0.678522649743967,-1.56771332720125,
0.817762781946031));
#6739=CARTESIAN_POINT('Ctrl Pts',(-0.621450160103226,-1.59241489490921,
0.821232225767726));
#6740=CARTESIAN_POINT('Ctrl Pts',(-0.563064313702586,-1.61397979088082,
0.82470166958942));
#6741=CARTESIAN_POINT('Ctrl Pts',(-0.503743386284735,-1.63228694268942,
0.828171113411115));
#6742=CARTESIAN_POINT('Ctrl Pts',(-0.443080327494135,-1.65100829238497,
0.831719053129651));
#6743=CARTESIAN_POINT('Ctrl Pts',(-0.381439894359464,-1.66632251886815,
0.835266992848186));
#6744=CARTESIAN_POINT('Ctrl Pts',(-0.319238175549031,-1.67815525198717,
0.838814932566722));
#6745=CARTESIAN_POINT('Ctrl Pts',(-0.257036456738598,-1.6899879851062,0.842362872285257));
#6746=CARTESIAN_POINT('Ctrl Pts',(-0.194274016137331,-1.69833921645597,
0.845910812003793));
#6747=CARTESIAN_POINT('Ctrl Pts',(-0.131370246528373,-1.70319109932711,
0.849458751722329));
#6748=CARTESIAN_POINT('Ctrl Pts',(-0.0697216369706872,-1.7079461694064,
0.852935897079466));
#6749=CARTESIAN_POINT('Ctrl Pts',(-0.00769170042111965,-1.70935926745733,
0.856413042436603));
#6750=CARTESIAN_POINT('Ctrl Pts',(0.0543269327415997,-1.70738591035503,
0.85989018779374));
#6751=CARTESIAN_POINT('Ctrl Pts',(0.116718177241874,-1.70540069721542,0.86338822403022));
#6752=CARTESIAN_POINT('Ctrl Pts',(0.179097471754126,-1.69998808811252,0.8668862602667));
#6753=CARTESIAN_POINT('Ctrl Pts',(0.241059829430328,-1.69115588315655,0.87038429650318));
#6754=CARTESIAN_POINT('Ctrl Pts',(0.302487049652064,-1.68239995747489,0.873852121974972));
#6755=CARTESIAN_POINT('Ctrl Pts',(0.363503994625234,-1.67028333183075,0.877319947446765));
#6756=CARTESIAN_POINT('Ctrl Pts',(0.423718594525157,-1.6548657393135,0.880787772918557));
#6757=CARTESIAN_POINT('Ctrl Pts',(0.483897359799761,-1.63945732204033,0.884253534634605));
#6758=CARTESIAN_POINT('Ctrl Pts',(0.543274236444688,-1.62075195929602,0.887719296350653));
#6759=CARTESIAN_POINT('Ctrl Pts',(0.601467916059901,-1.59886034676283,0.891185058066701));
#6760=CARTESIAN_POINT('Ctrl Pts',(0.65964816428865,-1.5769737869211,0.894650019867959));
#6761=CARTESIAN_POINT('Ctrl Pts',(0.716645283123954,-1.55190261607231,0.898114981669217));
#6762=CARTESIAN_POINT('Ctrl Pts',(0.772095624091946,-1.52380655260373,0.901579943470475));
#6763=CARTESIAN_POINT('Ctrl Pts',(0.8284575749594,-1.49524858666266,0.90510186963704));
#6764=CARTESIAN_POINT('Ctrl Pts',(0.883220929047204,-1.46356557419215,0.908623795803605));
#6765=CARTESIAN_POINT('Ctrl Pts',(0.93602962127879,-1.42897397127753,0.91214572197017));
#6766=CARTESIAN_POINT('Ctrl Pts',(0.988049100236263,-1.39489933159452,0.915615013792584));
#6767=CARTESIAN_POINT('Ctrl Pts',(1.03817156964567,-1.35800281172865,0.919084305614998));
#6768=CARTESIAN_POINT('Ctrl Pts',(1.08608788274937,-1.31853372101171,0.922553597437411));
#6769=CARTESIAN_POINT('Ctrl Pts',(1.1350946390228,-1.27816642261559,0.926101840776052));
#6770=CARTESIAN_POINT('Ctrl Pts',(1.18179315984421,-1.23510838225422,0.929650084114692));
#6771=CARTESIAN_POINT('Ctrl Pts',(1.22589239731985,-1.18966629467821,0.933198327453333));
#6772=CARTESIAN_POINT('Ctrl Pts',(1.2699916347955,-1.1442242071022,0.936746570791974));
#6773=CARTESIAN_POINT('Ctrl Pts',(1.31149127156381,-1.09639853899546,0.940294814130615));
#6774=CARTESIAN_POINT('Ctrl Pts',(1.35014567385118,-1.04652984758245,0.943843057469255));
#6775=CARTESIAN_POINT('Ctrl Pts',(1.38802379743077,-0.997662646324197,0.9473200430574));
#6776=CARTESIAN_POINT('Ctrl Pts',(1.42332100809394,-0.946638894748168,0.950797028645544));
#6777=CARTESIAN_POINT('Ctrl Pts',(1.45578418587916,-0.893761974266163,0.954274014233688));
#6778=CARTESIAN_POINT('Ctrl Pts',(1.48844409133214,-0.840564618326074,0.957772070441292));
#6779=CARTESIAN_POINT('Ctrl Pts',(1.51823512427273,-0.785491921303965,0.961270126648896));
#6780=CARTESIAN_POINT('Ctrl Pts',(1.54494099487746,-0.728886400509045,0.9647681828565));
#6781=CARTESIAN_POINT('Ctrl Pts',(1.57141478631477,-0.672772792609696,0.968235840280845));
#6782=CARTESIAN_POINT('Ctrl Pts',(1.59485659445252,-0.615153358056696,0.971703497705189));
#6783=CARTESIAN_POINT('Ctrl Pts',(1.61510063895128,-0.556388343299131,0.975171155129534));
#6784=CARTESIAN_POINT('Ctrl Pts',(1.6353326199887,-0.497658346716116,0.978636746170785));
#6785=CARTESIAN_POINT('Ctrl Pts',(1.65237045144827,-0.437784602479932,0.982102337212036));
#6786=CARTESIAN_POINT('Ctrl Pts',(1.66609683140508,-0.377146405102794,0.985567928253287));
#6787=CARTESIAN_POINT('Ctrl Pts',(1.6798200338144,-0.316522244984715,0.989032717037852));
#6788=CARTESIAN_POINT('Ctrl Pts',(1.6902331948799,-0.255134477737986,0.992497505822418));
#6789=CARTESIAN_POINT('Ctrl Pts',(1.69726966623695,-0.193374617186187,0.995962294606983));
#6790=CARTESIAN_POINT('Ctrl Pts',(1.7044225059232,-0.130593379381629,0.99948438365775));
#6791=CARTESIAN_POINT('Ctrl Pts',(1.70808584899727,-0.0674281599390935,
1.00300647270852));
#6792=CARTESIAN_POINT('Ctrl Pts',(1.70824459941817,-0.00429546954982385,
1.00652856175928));
#6793=CARTESIAN_POINT('Ctrl Pts',(1.70840096215087,0.0578876726139587,1.00999767677413));
#6794=CARTESIAN_POINT('Ctrl Pts',(1.70515753144939,0.120038744033914,1.01346679178899));
#6795=CARTESIAN_POINT('Ctrl Pts',(1.69855246280966,0.181762464725931,1.01693590680384));
#6796=CARTESIAN_POINT('Ctrl Pts',(1.6917961032174,0.244899984578319,1.02048448287256));
#6797=CARTESIAN_POINT('Ctrl Pts',(1.68152226277215,0.307589775897309,1.02403305894129));
#6798=CARTESIAN_POINT('Ctrl Pts',(1.66782702210342,0.36941993292409,1.02758163501001));
#6799=CARTESIAN_POINT('Ctrl Pts',(1.65413178143469,0.43125008995087,1.03113021107874));
#6800=CARTESIAN_POINT('Ctrl Pts',(1.6370153559103,0.492220090517584,1.03467878714746));
#6801=CARTESIAN_POINT('Ctrl Pts',(1.61662711611434,0.551937342407481,1.03822736321618));
#6802=CARTESIAN_POINT('Ctrl Pts',(1.59664941728707,0.610452117836267,1.04170448457027));
#6803=CARTESIAN_POINT('Ctrl Pts',(1.57345085609657,0.667997458907379,1.04518160592435));
#6804=CARTESIAN_POINT('Ctrl Pts',(1.54714561072322,0.724195085401638,1.04865872727843));
#6805=CARTESIAN_POINT('Ctrl Pts',(1.52068211661961,0.780730789070622,1.05215676651529));
#6806=CARTESIAN_POINT('Ctrl Pts',(1.49107453233224,0.835901995143896,1.05565480575215));
#6807=CARTESIAN_POINT('Ctrl Pts',(1.45848995386028,0.889339708429038,1.05915284498901));
#6808=CARTESIAN_POINT('Ctrl Pts',(1.42618707608989,0.942315441169128,1.06262064292298));
#6809=CARTESIAN_POINT('Ctrl Pts',(1.39095873370873,0.993587090027181,1.06608844085695));
#6810=CARTESIAN_POINT('Ctrl Pts',(1.35301463007387,1.04281804419854,1.06955623879092));
#6811=CARTESIAN_POINT('Ctrl Pts',(1.31509312141691,1.09201968229138,1.07302197171847));
#6812=CARTESIAN_POINT('Ctrl Pts',(1.27445936771176,1.13918263458369,1.07648770464602));
#6813=CARTESIAN_POINT('Ctrl Pts',(1.23136564333278,1.18400030190859,1.07995343757357));
#6814=CARTESIAN_POINT('Ctrl Pts',(1.18828188026439,1.22880760942565,1.08341836938118));
#6815=CARTESIAN_POINT('Ctrl Pts',(1.14273962708848,1.27127034289864,1.08688330118878));
#6816=CARTESIAN_POINT('Ctrl Pts',(1.09502922272576,1.31111748667944,1.09034823299639));
#6817=CARTESIAN_POINT('Ctrl Pts',(1.04653366466733,1.35162038118424,1.09387018599361));
#6818=CARTESIAN_POINT('Ctrl Pts',(0.99579833416888,1.38942043990573,1.09739213899084));
#6819=CARTESIAN_POINT('Ctrl Pts',(0.94316271883561,1.42427600846838,1.10091409198807));
#6820=CARTESIAN_POINT('Ctrl Pts',(0.8913146129287,1.45861008433772,1.10438335117394));
#6821=CARTESIAN_POINT('Ctrl Pts',(0.837623180639486,1.49008697865002,1.10785261035982));
#6822=CARTESIAN_POINT('Ctrl Pts',(0.782439547816649,1.51852112810869,1.1113218695457));
#6823=CARTESIAN_POINT('Ctrl Pts',(0.725998656982107,1.54760309758905,1.1148701694486));
#6824=CARTESIAN_POINT('Ctrl Pts',(0.667997234118838,1.57350171281687,1.1184184693515));
#6825=CARTESIAN_POINT('Ctrl Pts',(0.608832009473348,1.5960706897693,1.1219667692544));
#6826=CARTESIAN_POINT('Ctrl Pts',(0.549666784827857,1.61863966672173,1.12551506915731));
#6827=CARTESIAN_POINT('Ctrl Pts',(0.48933831255979,1.63787889810672,1.1290633690602));
#6828=CARTESIAN_POINT('Ctrl Pts',(0.428256500237485,1.65369720097252,1.13261166896311));
#6829=CARTESIAN_POINT('Ctrl Pts',(0.368400574695673,1.66919803702397,1.13608875595043));
#6830=CARTESIAN_POINT('Ctrl Pts',(0.307582676479223,1.68147584657023,1.13956584293775));
#6831=CARTESIAN_POINT('Ctrl Pts',(0.246181516856185,1.69041791378889,1.14304292992508));
#6832=CARTESIAN_POINT('Ctrl Pts',(0.184410289934603,1.69941387521215,1.14654097345778));
#6833=CARTESIAN_POINT('Ctrl Pts',(0.122049229967692,1.70503354944297,1.15003901699049));
#6834=CARTESIAN_POINT('Ctrl Pts',(0.0594984146863207,1.70721351949597,1.1535370605232));
#6835=CARTESIAN_POINT('Ctrl Pts',(-0.0025109364627393,1.70937461888217,
1.15700482363353));
#6836=CARTESIAN_POINT('Ctrl Pts',(-0.0647062559420003,1.70815530097898,
1.16047258674387));
#6837=CARTESIAN_POINT('Ctrl Pts',(-0.126691088671181,1.70354554695532,1.16394034985421));
#6838=CARTESIAN_POINT('Ctrl Pts',(-0.188639009003621,1.69893853807208,1.16740604788762));
#6839=CARTESIAN_POINT('Ctrl Pts',(-0.250376186231586,1.69094513465487,1.17087174592104));
#6840=CARTESIAN_POINT('Ctrl Pts',(-0.311507813255484,1.67960737816336,1.17433744395445));
#6841=CARTESIAN_POINT('Ctrl Pts',(-0.372625309096618,1.66827224250687,1.17780234085734));
#6842=CARTESIAN_POINT('Ctrl Pts',(-0.433137034075065,1.65359438129887,1.18126723776023));
#6843=CARTESIAN_POINT('Ctrl Pts',(-0.492656961259791,1.63566719751368,1.18473213466312));
#6844=CARTESIAN_POINT('Ctrl Pts',(-0.553157575290576,1.61744463444703,1.1882541213337));
#6845=CARTESIAN_POINT('Ctrl Pts',(-0.612632883565026,1.59586481638843,1.19177610800428));
#6846=CARTESIAN_POINT('Ctrl Pts',(-0.670694323999386,1.57107835140549,1.19529809467485));
#6847=CARTESIAN_POINT('Ctrl Pts',(-0.72788596043462,1.54666320629002,1.19876731933904));
#6848=CARTESIAN_POINT('Ctrl Pts',(-0.783705369257537,1.519137128998,1.20223654400323));
#6849=CARTESIAN_POINT('Ctrl Pts',(-0.837804453796072,1.4886912909329,1.20570576866742));
#6850=CARTESIAN_POINT('Ctrl Pts',(-0.893137694314755,1.45755089558574,1.20925413634119));
#6851=CARTESIAN_POINT('Ctrl Pts',(-0.946670663385841,1.42335615774327,1.21280250401496));
#6852=CARTESIAN_POINT('Ctrl Pts',(-0.998062955749583,1.3863579620215,1.21635087168873));
#6853=CARTESIAN_POINT('Ctrl Pts',(-1.04945524811332,1.34935976629973,1.2198992393625));
#6854=CARTESIAN_POINT('Ctrl Pts',(-1.09870646929954,1.30955851656066,1.22344760703627));
#6855=CARTESIAN_POINT('Ctrl Pts',(-1.14551498837387,1.26724641404536,1.22699597471004));
#6856=CARTESIAN_POINT('Ctrl Pts',(-1.1906986357399,1.22640309840167,1.23042116732171));
#6857=CARTESIAN_POINT('Ctrl Pts',(-1.23379799134156,1.18304695768846,1.23384635993338));
#6858=CARTESIAN_POINT('Ctrl Pts',(-1.27451524177969,1.13742206808698,1.23727155254505));
#6859=CARTESIAN_POINT('Ctrl Pts',(-1.31517768667276,1.09185858972806,1.24069213483686));
#6860=CARTESIAN_POINT('Ctrl Pts',(-1.35346402917097,1.04403279531404,1.24411271712868));
#6861=CARTESIAN_POINT('Ctrl Pts',(-1.38911118072363,0.994227433783946,1.2475332994205));
#6862=CARTESIAN_POINT('Ctrl Pts',(-1.42472427191129,0.944469660594528,1.25095061339279));
#6863=CARTESIAN_POINT('Ctrl Pts',(-1.45770286383511,0.892736490591282,1.25436792736509));
#6864=CARTESIAN_POINT('Ctrl Pts',(-1.4878237713354,0.839344081976698,1.25778524133739));
#6865=CARTESIAN_POINT('Ctrl Pts',(-1.51792765527182,0.785981849381159,1.26120062393153));
#6866=CARTESIAN_POINT('Ctrl Pts',(-1.54517679975331,0.730962692487708,1.26461600652567));
#6867=CARTESIAN_POINT('Ctrl Pts',(-1.56939228284869,0.67463021355034,1.26803138911981));
#6868=CARTESIAN_POINT('Ctrl Pts',(-1.59361608259122,0.618278387596485,1.27144794470447));
#6869=CARTESIAN_POINT('Ctrl Pts',(-1.61480392019255,0.560612814904588,1.27486450028913));
#6870=CARTESIAN_POINT('Ctrl Pts',(-1.63282439117922,0.501998575765123,1.27828105587378));
#6871=CARTESIAN_POINT('Ctrl Pts',(-1.65084729114232,0.443376436021646,1.28169807197542));
#6872=CARTESIAN_POINT('Ctrl Pts',(-1.66570183633137,0.383805881212224,1.28511508807706));
#6873=CARTESIAN_POINT('Ctrl Pts',(-1.67730691034948,0.323665863188982,1.28853210417871));
#6874=CARTESIAN_POINT('Ctrl Pts',(-1.68892792247905,0.263443250405129,1.29195381312275));
#6875=CARTESIAN_POINT('Ctrl Pts',(-1.69729047117641,0.202650131359429,1.2953755220668));
#6876=CARTESIAN_POINT('Ctrl Pts',(-1.70236506406829,0.141673043094835,1.29879723101085));
#6877=CARTESIAN_POINT('Ctrl Pts',(-1.70632609886975,0.09407664002299,1.30146808727392));
#6878=CARTESIAN_POINT('Ctrl Pts',(-1.70828490476063,0.0463683475638418,
1.304138943537));
#6879=CARTESIAN_POINT('Ctrl Pts',(-1.70824952897253,-0.00126856813606742,
1.30680979980007));
#6880=CARTESIAN_POINT('',(-1.70874899700092,0.00144479297225062,1.90680979980007));
#6881=CARTESIAN_POINT('Ctrl Pts',(-1.70952177679497,-0.00126951292371165,
1.30680979980007));
#6882=CARTESIAN_POINT('Ctrl Pts',(-1.71024375601734,-0.0879601103335736,
1.3116666266857));
#6883=CARTESIAN_POINT('Ctrl Pts',(-1.66510645419673,-0.73545936100502,1.34798488882031));
#6884=CARTESIAN_POINT('Ctrl Pts',(-0.83877314664564,-1.82974998182628,1.41576458620388));
#6885=CARTESIAN_POINT('Ctrl Pts',(1.0667458112657,-1.70692133093719,1.5101488919508));
#6886=CARTESIAN_POINT('Ctrl Pts',(2.01226847719202,-0.0479825385523114,
1.60453319769774));
#6887=CARTESIAN_POINT('Ctrl Pts',(1.14689041295175,1.65413688855294,1.69891750344466));
#6888=CARTESIAN_POINT('Ctrl Pts',(-0.750608607457775,1.86764917269852,1.79330180919158));
#6889=CARTESIAN_POINT('Ctrl Pts',(-1.64781001616314,0.790393313501198,1.86259924131006));
#6890=CARTESIAN_POINT('Ctrl Pts',(-1.70976669927472,0.115359128516567,1.90043523817955));
#6891=CARTESIAN_POINT('Ctrl Pts',(-1.70874899700092,0.00144479297225062,
1.90680979980007));
#6892=CARTESIAN_POINT('',(-1.705717720998,-0.000520512975719864,2.50680979980007));
#6893=CARTESIAN_POINT('Ctrl Pts',(-1.70874899700092,0.00144479297225062,
1.90680979980007));
#6894=CARTESIAN_POINT('Ctrl Pts',(-1.7047438638084,-0.446861256979479,1.93189667342853));
#6895=CARTESIAN_POINT('Ctrl Pts',(-1.29576946753668,-1.46386083145327,1.98844498230595));
#6896=CARTESIAN_POINT('Ctrl Pts',(0.411169349837819,-1.97039752822379,2.07645472643237));
#6897=CARTESIAN_POINT('Ctrl Pts',(1.87171845306621,-0.740403048133278,2.17083903217928));
#6898=CARTESIAN_POINT('Ctrl Pts',(1.6478520978538,1.15590228912575,2.26522333792622));
#6899=CARTESIAN_POINT('Ctrl Pts',(-0.0589656792105725,2.01197656350589,
2.35960764367313));
#6900=CARTESIAN_POINT('Ctrl Pts',(-1.46994986117608,1.19754152846963,2.44013646429776));
#6901=CARTESIAN_POINT('Ctrl Pts',(-1.7048382529488,0.315522270522238,2.4892038496734));
#6902=CARTESIAN_POINT('Ctrl Pts',(-1.705717720998,-0.000520512975719864,
2.50680979980007));
#6903=CARTESIAN_POINT('',(-1.71045989027119,-0.000789597318511919,3.10680979980007));
#6904=CARTESIAN_POINT('Ctrl Pts',(-1.705717720998,-0.000520512975719864,
2.50680979980007));
#6905=CARTESIAN_POINT('Ctrl Pts',(-1.70640984249009,-0.249239045816198,
2.52066528492238));
#6906=CARTESIAN_POINT('Ctrl Pts',(-1.53973233319606,-1.0618356879368,2.56598220529367));
#6907=CARTESIAN_POINT('Ctrl Pts',(-0.295068532255919,-1.99109547814598,
2.64276056091391));
#6908=CARTESIAN_POINT('Ctrl Pts',(1.50054859493888,-1.34159627149913,2.73714486666085));
#6909=CARTESIAN_POINT('Ctrl Pts',(1.94577713018251,0.515245573630572,2.83152917240776));
#6910=CARTESIAN_POINT('Ctrl Pts',(0.639942589016321,1.908402505851,2.9259134781547));
#6911=CARTESIAN_POINT('Ctrl Pts',(-1.18947887930053,1.59314638667863,3.01767368728545));
#6912=CARTESIAN_POINT('Ctrl Pts',(-1.70747901217689,0.513193512138237,3.07797246116726));
#6913=CARTESIAN_POINT('Ctrl Pts',(-1.71045989027119,-0.000789597318511919,
3.10680979980007));
#6914=CARTESIAN_POINT('',(-1.70758981783261,0.0014582535397993,3.70680979980007));
#6915=CARTESIAN_POINT('Ctrl Pts',(-1.71045989027119,-0.000789597318511919,
3.10680979980007));
#6916=CARTESIAN_POINT('Ctrl Pts',(-1.71073113971692,-0.0475602565482115,
3.10943389641623));
#6917=CARTESIAN_POINT('Ctrl Pts',(-1.68793010806937,-0.654816382704861,
3.1435194282814));
#6918=CARTESIAN_POINT('Ctrl Pts',(-0.964950165450157,-1.76646478021415,
3.20906639539542));
#6919=CARTESIAN_POINT('Ctrl Pts',(0.944491791186656,-1.77748752398191,3.30345070114242));
#6920=CARTESIAN_POINT('Ctrl Pts',(2.00395731635616,-0.188896044836109,3.3978350068893));
#6921=CARTESIAN_POINT('Ctrl Pts',(1.26000167422617,1.56968863870526,3.49221931263626));
#6922=CARTESIAN_POINT('Ctrl Pts',(-0.617867186307812,1.91566353559733,3.58660361838318));
#6923=CARTESIAN_POINT('Ctrl Pts',(-1.61963156293518,0.871340451104524,3.65813378077111));
#6924=CARTESIAN_POINT('Ctrl Pts',(-1.70888992723901,0.155539500215835,3.69820250791008));
#6925=CARTESIAN_POINT('Ctrl Pts',(-1.70758981783261,0.0014582535397993,
3.70680979980007));
#6926=CARTESIAN_POINT('',(-1.70629192088898,-0.00105167077536168,4.30680979980007));
#6927=CARTESIAN_POINT('Ctrl Pts',(-1.70758981783261,0.0014582535397993,
3.70680979980007));
#6928=CARTESIAN_POINT('Ctrl Pts',(-1.70413775798199,-0.407659381306412,
3.72966394315906));
#6929=CARTESIAN_POINT('Ctrl Pts',(-1.35288253689885,-1.38529989117204,3.78397952176701));
#6930=CARTESIAN_POINT('Ctrl Pts',(0.272061413425965,-1.99436938124897,3.86975653562395));
#6931=CARTESIAN_POINT('Ctrl Pts',(1.81522410712393,-0.869763233554926,3.96414084137088));
#6932=CARTESIAN_POINT('Ctrl Pts',(1.72481229728226,1.03756887996144,4.05852514711779));
#6933=CARTESIAN_POINT('Ctrl Pts',(0.0821902775978209,2.01116170405157,4.15290945286473));
#6934=CARTESIAN_POINT('Ctrl Pts',(-1.42301171001672,1.27783575536462,4.23567100375882));
#6935=CARTESIAN_POINT('Ctrl Pts',(-1.70424737531169,0.354769758201447,4.28697111940393));
#6936=CARTESIAN_POINT('Ctrl Pts',(-1.70629192088898,-0.00105167077536168,
4.30680979980007));
#6937=CARTESIAN_POINT('',(-1.71092577309385,-0.00012504919473697,4.90680979980007));
#6938=CARTESIAN_POINT('Ctrl Pts',(-1.70629192088898,-0.00105167077536168,
4.30680979980007));
#6939=CARTESIAN_POINT('Ctrl Pts',(-1.70748974511699,-0.209514388950238,
4.31843255465291));
#6940=CARTESIAN_POINT('Ctrl Pts',(-1.57615353051455,-0.980804623883353,
4.3615167447547));
#6941=CARTESIAN_POINT('Ctrl Pts',(-0.43389044046669,-1.96551920048943,4.4360623701055));
#6942=CARTESIAN_POINT('Ctrl Pts',(1.40283186881175,-1.44346437052995,4.53044667585243));
#6943=CARTESIAN_POINT('Ctrl Pts',(1.97710379266664,0.377607248774025,4.62483098159934));
#6944=CARTESIAN_POINT('Ctrl Pts',(0.7721208389405,1.85885880407731,4.71921528734628));
#6945=CARTESIAN_POINT('Ctrl Pts',(-1.11983905399775,1.66806212057561,4.81320822674652));
#6946=CARTESIAN_POINT('Ctrl Pts',(-1.71033251354333,0.553250797363694,4.87573973089778));
#6947=CARTESIAN_POINT('Ctrl Pts',(-1.71092577309385,-0.00012504919473697,
4.90680979980007));
#6948=CARTESIAN_POINT('',(-1.70658039029172,0.00119792360719225,5.50680979980008));
#6949=CARTESIAN_POINT('Ctrl Pts',(-1.71092577309385,-0.00012504919473697,
4.90680979980007));
#6950=CARTESIAN_POINT('Ctrl Pts',(-1.7109332459393,-0.0070955095465335,
4.90720116614676));
#6951=CARTESIAN_POINT('Ctrl Pts',(-1.71089426063458,-0.0140658840322902,
4.90759253249344));
#6952=CARTESIAN_POINT('Ctrl Pts',(-1.70391933284558,-0.581328914761308,
4.9394453340891));
#6953=CARTESIAN_POINT('Ctrl Pts',(-1.08638139435793,-1.69449169943945,5.00236820458706));
#6954=CARTESIAN_POINT('Ctrl Pts',(0.817592645828785,-1.8393120678936,5.09675251033397));
#6955=CARTESIAN_POINT('Ctrl Pts',(1.98579059287652,-0.328880479199768,5.19113681608091));
#6956=CARTESIAN_POINT('Ctrl Pts',(1.3669161520747,1.47752054032031,5.28552112182784));
#6957=CARTESIAN_POINT('Ctrl Pts',(-0.482087048092087,1.95425651935824,5.37990542757475));
#6958=CARTESIAN_POINT('Ctrl Pts',(-1.58805687488604,0.95238534644948,5.45366832023218));
#6959=CARTESIAN_POINT('Ctrl Pts',(-1.70786729365446,0.195538944080348,5.49596977764062));
#6960=CARTESIAN_POINT('Ctrl Pts',(-1.70658039029172,0.00119792360719225,
5.50680979980008));
#6961=CARTESIAN_POINT('',(-1.70721003800208,-0.00139829312648681,6.10680979980007));
#6962=CARTESIAN_POINT('Ctrl Pts',(-1.70658039029172,0.00119792360719225,
5.50680979980008));
#6963=CARTESIAN_POINT('Ctrl Pts',(-1.70413226191533,-0.368504868920307,
5.52743121288959));
#6964=CARTESIAN_POINT('Ctrl Pts',(-1.40556429020907,-1.30585481825115,5.57951406122808));
#6965=CARTESIAN_POINT('Ctrl Pts',(0.131615469299055,-2.00853248810358,5.66305834481553));
#6966=CARTESIAN_POINT('Ctrl Pts',(1.74980235607298,-0.99484646099087,5.75744265056247));
#6967=CARTESIAN_POINT('Ctrl Pts',(1.79328979108982,0.914133772091395,5.85182695630937));
#6968=CARTESIAN_POINT('Ctrl Pts',(0.222941955990293,2.00045366742654,5.94621126205633));
#6969=CARTESIAN_POINT('Ctrl Pts',(-1.37184809092268,1.35754094959989,6.03120554321987));
#6970=CARTESIAN_POINT('Ctrl Pts',(-1.70407444749312,0.393931601296323,6.08473838913446));
#6971=CARTESIAN_POINT('Ctrl Pts',(-1.70721003800208,-0.00139829312648681,
6.10680979980007));
#6972=CARTESIAN_POINT('',(-1.71069332253564,0.000492187094742366,6.70680979980008));
#6973=CARTESIAN_POINT('Ctrl Pts',(-1.70721003800208,-0.00139829312648681,
6.10680979980007));
#6974=CARTESIAN_POINT('Ctrl Pts',(-1.70854403846125,-0.169586791968197,
6.11619982438344));
#6975=CARTESIAN_POINT('Ctrl Pts',(-1.60895730772148,-0.899747975566428,
6.15705128421577));
#6976=CARTESIAN_POINT('Ctrl Pts',(-0.570578023721532,-1.93026152129124,
6.22936417929709));
#6977=CARTESIAN_POINT('Ctrl Pts',(1.29821511874949,-1.53826168179717,6.32374848504401));
#6978=CARTESIAN_POINT('Ctrl Pts',(1.9987084670187,0.238165610479905,6.41813279079093));
#6979=CARTESIAN_POINT('Ctrl Pts',(0.900498826589758,1.8000707639935,6.51251709653787));
#6980=CARTESIAN_POINT('Ctrl Pts',(-1.00808634131497,1.74239953938573,6.60690140228478));
#6981=CARTESIAN_POINT('Ctrl Pts',(-1.69522136426491,0.626405574154833,6.67166563670553));
#6982=CARTESIAN_POINT('Ctrl Pts',(-1.71083804055838,0.0332932687764938,
6.70496843587729));
#6983=CARTESIAN_POINT('Ctrl Pts',(-1.71069332253564,0.000492187094742366,
6.70680979980008));
#6984=CARTESIAN_POINT('',(0.433376258375141,-1.65493082312738,6.88122480138927));
#6985=CARTESIAN_POINT('Ctrl Pts',(-1.71069332253564,0.000492187094742366,
6.70680979980008));
#6986=CARTESIAN_POINT('Ctrl Pts',(-1.70836539696767,-0.527144075876519,
6.73642987112627));
#6987=CARTESIAN_POINT('Ctrl Pts',(-1.19174755964131,-1.566331294562,6.79456820498932));
#6988=CARTESIAN_POINT('Ctrl Pts',(-0.0592995318133123,-1.78055737442536,
6.85270653885239));
#6989=CARTESIAN_POINT('Ctrl Pts',(0.433376258375141,-1.65493082312738,6.88122480138927));
#6990=CARTESIAN_POINT('',(-1.03231334037779,-1.36104637311814,6.88122480138927));
#6991=CARTESIAN_POINT('Origin',(0.,0.,6.88122480138927));
#6992=CARTESIAN_POINT('',(-1.7090644143042,0.000376576228701876,6.79319020019992));
#6993=CARTESIAN_POINT('Ctrl Pts',(-1.03231334037779,-1.36104637311814,6.88122480138927));
#6994=CARTESIAN_POINT('Ctrl Pts',(-1.08459431799775,-1.32139280090265,6.87755669300638));
#6995=CARTESIAN_POINT('Ctrl Pts',(-1.13464020645309,-1.27868275150367,6.87388858462349));
#6996=CARTESIAN_POINT('Ctrl Pts',(-1.18208844104253,-1.23320111095216,6.8702204762406));
#6997=CARTESIAN_POINT('Ctrl Pts',(-1.22757216456718,-1.18960255808308,6.86670423946194));
#6998=CARTESIAN_POINT('Ctrl Pts',(-1.27066873038283,-1.14345778921077,6.86318800268328));
#6999=CARTESIAN_POINT('Ctrl Pts',(-1.31109333933297,-1.09505813455575,6.85967176590462));
#7000=CARTESIAN_POINT('Ctrl Pts',(-1.35150659787644,-1.04667206953777,6.85615651641362));
#7001=CARTESIAN_POINT('Ctrl Pts',(-1.38924907585107,-0.996032750533164,
6.85264126692262));
#7002=CARTESIAN_POINT('Ctrl Pts',(-1.42407536961439,-0.94346563485781,6.84912601743161));
#7003=CARTESIAN_POINT('Ctrl Pts',(-1.45890322424902,-0.890896163189488,
6.84561061039149));
#7004=CARTESIAN_POINT('Ctrl Pts',(-1.49081436599465,-0.836399131200913,
6.84209520335136));
#7005=CARTESIAN_POINT('Ctrl Pts',(-1.51960696700599,-0.78032860278658,6.83857979631123));
#7006=CARTESIAN_POINT('Ctrl Pts',(-1.54841023310964,-0.7242373052392,6.83506308712613));
#7007=CARTESIAN_POINT('Ctrl Pts',(-1.5740924429493,-0.666571789194321,6.83154637794103));
#7008=CARTESIAN_POINT('Ctrl Pts',(-1.59649873557777,-0.60770868826978,6.82802966875593));
#7009=CARTESIAN_POINT('Ctrl Pts',(-1.61893717283678,-0.548761140861256,
6.82450791441146));
#7010=CARTESIAN_POINT('Ctrl Pts',(-1.63809014229962,-0.488613038233603,
6.82098616006698));
#7011=CARTESIAN_POINT('Ctrl Pts',(-1.65385207374626,-0.42765801835719,6.8174644057225));
#7012=CARTESIAN_POINT('Ctrl Pts',(-1.66962716398094,-0.3666521104161,6.8139397112549));
#7013=CARTESIAN_POINT('Ctrl Pts',(-1.68200548521952,-0.304838423128845,
6.81041501678731));
#7014=CARTESIAN_POINT('Ctrl Pts',(-1.69093278872226,-0.242619798293478,
6.80689032231972));
#7015=CARTESIAN_POINT('Ctrl Pts',(-1.69987711779078,-0.180282514191069,
6.80335890578677));
#7016=CARTESIAN_POINT('Ctrl Pts',(-1.70535725198845,-0.117539237435382,
6.79982748925383));
#7017=CARTESIAN_POINT('Ctrl Pts',(-1.70737092020885,-0.0547960155959329,
6.79629607272089));
#7018=CARTESIAN_POINT('Ctrl Pts',(-1.70796125902744,-0.0364018436661475,
6.79526078188056));
#7019=CARTESIAN_POINT('Ctrl Pts',(-1.70825400928489,-0.0180076557448326,
6.79422549104024));
#7020=CARTESIAN_POINT('Ctrl Pts',(-1.70824995853226,0.000376396771052057,
6.79319020019992));
#7021=CARTESIAN_POINT('',(-1.70733856330343,-0.0014377884632695,6.19319020019993));
#7022=CARTESIAN_POINT('Ctrl Pts',(-1.71055216417171,0.000376904040357041,
6.79319020019992));
#7023=CARTESIAN_POINT('Ctrl Pts',(-1.71073076079401,0.0380123029285045,
6.79107363201406));
#7024=CARTESIAN_POINT('Ctrl Pts',(-1.69251520158208,0.635023283971082,6.75749562857924));
#7025=CARTESIAN_POINT('Ctrl Pts',(-0.99317638825687,1.75221471014715,6.69245618989542));
#7026=CARTESIAN_POINT('Ctrl Pts',(0.916129322380027,1.79161764679409,6.5980718841485));
#7027=CARTESIAN_POINT('Ctrl Pts',(2.00063946484888,0.221190637255988,6.50368757840157));
#7028=CARTESIAN_POINT('Ctrl Pts',(1.28489523215748,-1.54959303984541,6.40930327265464));
#7029=CARTESIAN_POINT('Ctrl Pts',(-0.587259843124623,-1.92516956402138,
6.31491896690772));
#7030=CARTESIAN_POINT('Ctrl Pts',(-1.61275586842781,-0.889773899116702,
6.24288127608948));
#7031=CARTESIAN_POINT('Ctrl Pts',(-1.70866489019705,-0.164666545902499,
6.20230502052022));
#7032=CARTESIAN_POINT('Ctrl Pts',(-1.70733856330343,-0.0014377884632695,
6.19319020019993));
#7033=CARTESIAN_POINT('',(-1.70647429782816,0.00114928838020923,5.59319020019992));
#7034=CARTESIAN_POINT('Ctrl Pts',(-1.70733856330343,-0.0014377884632695,
6.19319020019993));
#7035=CARTESIAN_POINT('Ctrl Pts',(-1.70408683531321,0.398746752713406,6.17084358527124));
#7036=CARTESIAN_POINT('Ctrl Pts',(-1.3652449466822,1.36733416363711,6.11703553509359));
#7037=CARTESIAN_POINT('Ctrl Pts',(0.240231051783908,1.99843873469232,6.03176604966692));
#7038=CARTESIAN_POINT('Ctrl Pts',(1.80112487550057,0.898601953609902,5.93738174392003));
#7039=CARTESIAN_POINT('Ctrl Pts',(1.74113633374771,-1.0099409559506,5.84299743817307));
#7040=CARTESIAN_POINT('Ctrl Pts',(0.114245086704342,-2.00959340467034,5.74861313242617));
#7041=CARTESIAN_POINT('Ctrl Pts',(-1.41175815753826,-1.29601290328604,5.66534405310177));
#7042=CARTESIAN_POINT('Ctrl Pts',(-1.70416640047656,-0.363676910033684,
5.61353640902636));
#7043=CARTESIAN_POINT('Ctrl Pts',(-1.70647429782816,0.00114928838020924,
5.59319020019992));
#7044=CARTESIAN_POINT('',(-1.71093671904409,-3.71626710015116E-5,4.99319020019992));
#7045=CARTESIAN_POINT('Ctrl Pts',(-1.70647429782816,0.00114928838020922,
5.59319020019992));
#7046=CARTESIAN_POINT('Ctrl Pts',(-1.70773511264835,0.200455499912553,5.58207497377739));
#7047=CARTESIAN_POINT('Ctrl Pts',(-1.58392193718951,0.962377793456982,5.53949831210587));
#7048=CARTESIAN_POINT('Ctrl Pts',(-0.465173068895533,1.95835109737102,5.46546021518539));
#7049=CARTESIAN_POINT('Ctrl Pts',(1.37963915910134,1.46564745709577,5.37107590943847));
#7050=CARTESIAN_POINT('Ctrl Pts',(1.98287289578746,-0.346036772783098,5.27669160369153));
#7051=CARTESIAN_POINT('Ctrl Pts',(0.801659924002396,-1.84631185111647,5.18230729794462));
#7052=CARTESIAN_POINT('Ctrl Pts',(-1.10099078479098,-1.68503579381714,5.08792299219768));
#7053=CARTESIAN_POINT('Ctrl Pts',(-1.71000378738849,-0.56451081151032,5.02488395961612));
#7054=CARTESIAN_POINT('Ctrl Pts',(-1.71093739349098,-0.00210604024018896,
4.99330636228354));
#7055=CARTESIAN_POINT('Ctrl Pts',(-1.71093671904409,-3.71626710014006E-5,
4.99319020019992));
#7056=CARTESIAN_POINT('',(-1.70638863318681,-0.00110593147553267,4.39319020019992));
#7057=CARTESIAN_POINT('Ctrl Pts',(-1.71093671904409,-3.71626710016226E-5,
4.99319020019992));
#7058=CARTESIAN_POINT('Ctrl Pts',(-1.71075472573678,0.558230479703889,4.96184492703456));
#7059=CARTESIAN_POINT('Ctrl Pts',(-1.11091973990757,1.67717074904876,4.89903821862023));
#7060=CARTESIAN_POINT('Ctrl Pts',(0.788163059251489,1.85211372924192,4.8047700749569));
#7061=CARTESIAN_POINT('Ctrl Pts',(1.9802944814926,0.360499692491619,4.71038576920999));
#7062=CARTESIAN_POINT('Ctrl Pts',(1.39029962886282,-1.45553880087964,4.61600146346305));
#7063=CARTESIAN_POINT('Ctrl Pts',(-0.450867470888686,-1.96169436651404,
4.52161715771613));
#7064=CARTESIAN_POINT('Ctrl Pts',(-1.58038891107441,-0.970812636144332,
4.44734673662842));
#7065=CARTESIAN_POINT('Ctrl Pts',(-1.70762300397305,-0.204603575060088,
4.40453775078968));
#7066=CARTESIAN_POINT('Ctrl Pts',(-1.70638863318681,-0.00110593147553267,
4.39319020019992));
#7067=CARTESIAN_POINT('',(-1.70745364674527,0.00144013658803385,3.79319020019992));
#7068=CARTESIAN_POINT('Ctrl Pts',(-1.70638863318681,-0.00110593147553267,
4.39319020019992));
#7069=CARTESIAN_POINT('Ctrl Pts',(-1.70420067276091,0.359599940607081,4.37307631554071));
#7070=CARTESIAN_POINT('Ctrl Pts',(-1.41693678240365,1.28769571311434,4.32150099563251));
#7071=CARTESIAN_POINT('Ctrl Pts',(0.0995750801122244,2.01037585185725,4.23846424047536));
#7072=CARTESIAN_POINT('Ctrl Pts',(1.73371824985778,1.02261786219037,4.14407993472842));
#7073=CARTESIAN_POINT('Ctrl Pts',(1.80763647646394,-0.88542454841268,4.04969562898151));
#7074=CARTESIAN_POINT('Ctrl Pts',(0.254808535468846,-1.99664690727106,3.95531132323457));
#7075=CARTESIAN_POINT('Ctrl Pts',(-1.3596124526819,-1.37555056956786,3.86980951364072));
#7076=CARTESIAN_POINT('Ctrl Pts',(-1.70410728468879,-0.402832987616667,
3.81576913929583));
#7077=CARTESIAN_POINT('Ctrl Pts',(-1.70745364674527,0.00144013658803385,
3.79319020019992));
#7078=CARTESIAN_POINT('',(-1.71054831940743,-0.000715229540035611,3.19319020019992));
#7079=CARTESIAN_POINT('Ctrl Pts',(-1.70745364674527,0.00144013658803385,
3.79319020019992));
#7080=CARTESIAN_POINT('Ctrl Pts',(-1.70877009691005,0.160480136442858,3.78430770404685));
#7081=CARTESIAN_POINT('Ctrl Pts',(-1.61592638481939,0.881326231316457,3.74396377264484));
#7082=CARTESIAN_POINT('Ctrl Pts',(-0.601281834025254,1.92093373599865,3.67215840599379));
#7083=CARTESIAN_POINT('Ctrl Pts',(1.27352556254399,1.55873631623992,3.57777410024688));
#7084=CARTESIAN_POINT('Ctrl Pts',(2.00224918884281,-0.206214567376117,3.48338979449994));
#7085=CARTESIAN_POINT('Ctrl Pts',(0.929088842915232,-1.78558678982326,3.38900548875303));
#7086=CARTESIAN_POINT('Ctrl Pts',(-0.980186360320026,-1.75805601761238,
3.29462118300609));
#7087=CARTESIAN_POINT('Ctrl Pts',(-1.69053325787773,-0.644891975364033,
3.22934942015507));
#7088=CARTESIAN_POINT('Ctrl Pts',(-1.71077187969281,-0.042575030137566,
3.19553909255301));
#7089=CARTESIAN_POINT('Ctrl Pts',(-1.71054831940743,-0.000715229540035611,
3.19319020019992));
#7090=CARTESIAN_POINT('',(-1.70576661654484,-0.000592994286356119,2.59319020019992));
#7091=CARTESIAN_POINT('Ctrl Pts',(-1.71054831940743,-0.000715229540035611,
3.19319020019992));
#7092=CARTESIAN_POINT('Ctrl Pts',(-1.70777747791287,0.518101751965672,3.16407765730403));
#7093=CARTESIAN_POINT('Ctrl Pts',(-1.18115523050738,1.60247259901729,3.10350367915917));
#7094=CARTESIAN_POINT('Ctrl Pts',(0.656418095559625,1.90279834608092,3.01146826576533));
#7095=CARTESIAN_POINT('Ctrl Pts',(1.95015896916594,0.498403708851651,2.91708396001839));
#7096=CARTESIAN_POINT('Ctrl Pts',(1.48889341829145,-1.35451934315334,2.82269965427146));
#7097=CARTESIAN_POINT('Ctrl Pts',(-0.312271882189301,-1.98846989759894,
2.72831534852454));
#7098=CARTESIAN_POINT('Ctrl Pts',(-1.54442260766096,-1.05185319082121,2.65181219716736));
#7099=CARTESIAN_POINT('Ctrl Pts',(-1.7065407794744,-0.244353809801757,2.60677048105915));
#7100=CARTESIAN_POINT('Ctrl Pts',(-1.70576661654484,-0.000592994286356119,
2.59319020019992));
#7101=CARTESIAN_POINT('',(-1.7086043211043,0.00146224045955247,1.99319020019992));
#7102=CARTESIAN_POINT('Ctrl Pts',(-1.70576661654484,-0.000592994286356119,
2.59319020019992));
#7103=CARTESIAN_POINT('Ctrl Pts',(-1.70474727629631,0.320366846057213,2.57530904581018));
#7104=CARTESIAN_POINT('Ctrl Pts',(-1.46438715133716,1.20746393579915,2.52596645617147));
#7105=CARTESIAN_POINT('Ctrl Pts',(-0.041568549553779,2.01241107082974,2.44516243128376));
#7106=CARTESIAN_POINT('Ctrl Pts',(1.65778400451944,1.14161221786942,2.35077812553685));
#7107=CARTESIAN_POINT('Ctrl Pts',(1.8652471156411,-0.756557637845384,2.25639381978991));
#7108=CARTESIAN_POINT('Ctrl Pts',(0.394118520517271,-1.97387863246546,2.16200951404299));
#7109=CARTESIAN_POINT('Ctrl Pts',(-1.30305340392856,-1.45423325181973,2.07427497417966));
#7110=CARTESIAN_POINT('Ctrl Pts',(-1.70463207257213,-0.442022540533928,
2.0180018695653));
#7111=CARTESIAN_POINT('Ctrl Pts',(-1.7086043211043,0.00146224045955247,
1.99319020019992));
#7112=CARTESIAN_POINT('',(-1.70965372155593,-0.00122376277469999,1.39319020019992));
#7113=CARTESIAN_POINT('Ctrl Pts',(-1.7086043211043,0.00146224045955247,
1.99319020019992));
#7114=CARTESIAN_POINT('Ctrl Pts',(-1.70966892189281,0.120320424611316,1.98654043431633));
#7115=CARTESIAN_POINT('Ctrl Pts',(-1.64451481097969,0.800362997705775,1.94842923318373));
#7116=CARTESIAN_POINT('Ctrl Pts',(-0.734433412509021,1.8740687918552,1.87885659680224));
#7117=CARTESIAN_POINT('Ctrl Pts',(1.16114866158118,1.64415936688714,1.78447229105527));
#7118=CARTESIAN_POINT('Ctrl Pts',(2.01177830590373,-0.0653782589161231,
1.69008798530838));
#7119=CARTESIAN_POINT('Ctrl Pts',(1.05194843294444,-1.7160800765306,1.59570367956143));
#7120=CARTESIAN_POINT('Ctrl Pts',(-0.854561305477856,-1.82242998781983,
1.50131937381452));
#7121=CARTESIAN_POINT('Ctrl Pts',(-1.66808598891422,-0.725507541111736,
1.433814880694));
#7122=CARTESIAN_POINT('Ctrl Pts',(-1.71031813974082,-0.0829856766656713,
1.39777182282248));
#7123=CARTESIAN_POINT('Ctrl Pts',(-1.70965372155593,-0.00122376277469999,
1.39319020019992));
#7124=CARTESIAN_POINT('',(-1.70798406265114,2.48985917316355E-5,0.793190198053302));
#7125=CARTESIAN_POINT('Ctrl Pts',(-1.70965372155593,-0.00122376277469999,
1.39319020019992));
#7126=CARTESIAN_POINT('Ctrl Pts',(-1.70575566233395,0.47846326219923,1.3663103875735));
#7127=CARTESIAN_POINT('Ctrl Pts',(-1.24660295336588,1.52614216487693,1.3079691396981));
#7128=CARTESIAN_POINT('Ctrl Pts',(0.521444772704797,1.9441245725567,1.21816645657374));
#7129=CARTESIAN_POINT('Ctrl Pts',(1.91043254963484,0.633857130546934,1.1237821508268));
#7130=CARTESIAN_POINT('Ctrl Pts',(1.5801645446874,-1.24683939123611,1.02939784507989));
#7131=CARTESIAN_POINT('Ctrl Pts',(-0.172140159774847,-2.00546387584604,
0.935013539332954));
#7132=CARTESIAN_POINT('Ctrl Pts',(-1.50469283484901,-1.13276427476656,0.856277657706305));
#7133=CARTESIAN_POINT('Ctrl Pts',(-1.70552555931313,-0.283899278264277,
0.809003211328624));
#7134=CARTESIAN_POINT('Ctrl Pts',(-1.7055606080675,2.48247144564451E-5,
0.793190200199919));
#7135=CARTESIAN_POINT('Ctrl Pts',(-1.70824999981843,2.49066986354841E-5,
0.793190197817743));
#7136=CARTESIAN_POINT('Ctrl Pts',(-1.70824904800449,0.0653059853313177,
0.789560124769425));
#7137=CARTESIAN_POINT('Ctrl Pts',(-1.70450170914895,0.130515412064531,0.785930051721107));
#7138=CARTESIAN_POINT('Ctrl Pts',(-1.69705822465692,0.195221527051415,0.782299978672789));
#7139=CARTESIAN_POINT('Ctrl Pts',(-1.68959377517735,0.260109890405459,0.778659681322087));
#7140=CARTESIAN_POINT('Ctrl Pts',(-1.67841243357824,0.324491680054332,0.775019383971384));
#7141=CARTESIAN_POINT('Ctrl Pts',(-1.66361588672389,0.387943609226772,0.771379086620682));
#7142=CARTESIAN_POINT('Ctrl Pts',(-1.64879657993075,0.45149313968672,0.767733189791556));
#7143=CARTESIAN_POINT('Ctrl Pts',(-1.63035110565223,0.514109545100054,0.764087292962431));
#7144=CARTESIAN_POINT('Ctrl Pts',(-1.60843066443068,0.575385835956247,0.760441396133305));
#7145=CARTESIAN_POINT('Ctrl Pts',(-1.58645287966122,0.636822424677127,0.756785961692349));
#7146=CARTESIAN_POINT('Ctrl Pts',(-1.5609821340813,0.696911497006324,0.753130527251392));
#7147=CARTESIAN_POINT('Ctrl Pts',(-1.53221724143077,0.755267096835475,0.749475092810436));
#7148=CARTESIAN_POINT('Ctrl Pts',(-1.52374443652028,0.772455953362547,0.748398371153326));
#7149=CARTESIAN_POINT('Ctrl Pts',(-1.5149861191257,0.789494590766846,0.747321649496215));
#7150=CARTESIAN_POINT('Ctrl Pts',(-1.50594809069531,0.806373617271273,0.746244927839105));
#7151=CARTESIAN_POINT('Ctrl Pts',(-1.47676075081638,0.860882616352725,0.742767771155749));
#7152=CARTESIAN_POINT('Ctrl Pts',(-1.44455193799279,0.913913534313018,0.739290614472393));
#7153=CARTESIAN_POINT('Ctrl Pts',(-1.40949556232082,0.965111559509007,0.735813457789037));
#7154=CARTESIAN_POINT('Ctrl Pts',(-1.37422869517758,1.01661699662204,0.732315422968335));
#7155=CARTESIAN_POINT('Ctrl Pts',(-1.33608013502565,1.0662669659466,0.728817388147633));
#7156=CARTESIAN_POINT('Ctrl Pts',(-1.29527450114133,1.11372439552749,0.72531935332693));
#7157=CARTESIAN_POINT('Ctrl Pts',(-1.25482121350369,1.16077204230149,0.721851523145208));
#7158=CARTESIAN_POINT('Ctrl Pts',(-1.21175688544118,1.2056644663069,0.718383692963486));
#7159=CARTESIAN_POINT('Ctrl Pts',(-1.16634294648347,1.24810343869739,0.714915862781763));
#7160=CARTESIAN_POINT('Ctrl Pts',(-1.12095606655812,1.29051712463281,0.711450098840743));
#7161=CARTESIAN_POINT('Ctrl Pts',(-1.07322272201843,1.33047991231744,0.707984334899722));
#7162=CARTESIAN_POINT('Ctrl Pts',(-1.02344149396535,1.36773007970505,0.704518570958701));
#7163=CARTESIAN_POINT('Ctrl Pts',(-0.973671791295235,1.40497162290917,0.70105360941365));
#7164=CARTESIAN_POINT('Ctrl Pts',(-0.921855552555898,1.43950148904052,0.697588647868598));
#7165=CARTESIAN_POINT('Ctrl Pts',(-0.868323161565795,1.47109923172721,0.694123686323547));
#7166=CARTESIAN_POINT('Ctrl Pts',(-0.813910752042225,1.50321640944502,0.690601764304266));
#7167=CARTESIAN_POINT('Ctrl Pts',(-0.757725698401431,1.53230387803247,0.687079842284985));
#7168=CARTESIAN_POINT('Ctrl Pts',(-0.700142113430193,1.55817812958002,0.683557920265704));
#7169=CARTESIAN_POINT('Ctrl Pts',(-0.643419138270495,1.58366568004325,0.680088634785931));
#7170=CARTESIAN_POINT('Ctrl Pts',(-0.585339659884467,1.60603528705814,0.676619349306157));
#7171=CARTESIAN_POINT('Ctrl Pts',(-0.526280215216498,1.62516066823304,0.673150063826383));
#7172=CARTESIAN_POINT('Ctrl Pts',(-0.465876681912426,1.64472130929979,0.669601823537349));
#7173=CARTESIAN_POINT('Ctrl Pts',(-0.404448563601747,1.66088807131683,0.666053583248315));
#7174=CARTESIAN_POINT('Ctrl Pts',(-0.342411013067568,1.673580819868,0.662505342959281));
#7175=CARTESIAN_POINT('Ctrl Pts',(-0.280373462533389,1.68627356841916,0.658957102670247));
#7176=CARTESIAN_POINT('Ctrl Pts',(-0.217727043916524,1.69549228730872,0.655408862381214));
#7177=CARTESIAN_POINT('Ctrl Pts',(-0.15489099546036,1.70121334406514,0.651860622092181));
#7178=CARTESIAN_POINT('Ctrl Pts',(-0.0933111593584229,1.70682002599448,
0.648383317888346));
#7179=CARTESIAN_POINT('Ctrl Pts',(-0.0313038835783991,1.70909001322935,
0.64490601368451));
#7180=CARTESIAN_POINT('Ctrl Pts',(0.0307388207184475,1.70797341530858,0.641428709480675));
#7181=CARTESIAN_POINT('Ctrl Pts',(0.0931510755020205,1.70685016649613,0.637930693100032));
#7182=CARTESIAN_POINT('Ctrl Pts',(0.155598673626593,1.70229973564838,0.634432676719391));
#7183=CARTESIAN_POINT('Ctrl Pts',(0.217676590514528,1.69432433862055,0.630934660338748));
#7184=CARTESIAN_POINT('Ctrl Pts',(0.279221525684353,1.6864174158751,0.627466676840554));
#7185=CARTESIAN_POINT('Ctrl Pts',(0.340402590208932,1.67514416271573,0.62399869334236));
#7186=CARTESIAN_POINT('Ctrl Pts',(0.400826897536886,1.6605589001029,0.620530709844166));
#7187=CARTESIAN_POINT('Ctrl Pts',(0.461215233697022,1.64598232023634,0.617064790869702));
#7188=CARTESIAN_POINT('Ctrl Pts',(0.520847213960595,1.62809775984405,0.613598871895239));
#7189=CARTESIAN_POINT('Ctrl Pts',(0.579340008693228,1.60701064614623,0.610132952920775));
#7190=CARTESIAN_POINT('Ctrl Pts',(0.637819286059113,1.5859284055657,0.606667834901337));
#7191=CARTESIAN_POINT('Ctrl Pts',(0.695159423647654,1.56164525319152,0.6032027168819));
#7192=CARTESIAN_POINT('Ctrl Pts',(0.750994572684008,1.534315878266,0.599737598862462));
#7193=CARTESIAN_POINT('Ctrl Pts',(0.807742640007617,1.50653966140347,0.596215825319362));
#7194=CARTESIAN_POINT('Ctrl Pts',(0.862935559076709,1.47561691060882,0.59269405177626));
#7195=CARTESIAN_POINT('Ctrl Pts',(0.916214371241624,1.44175909514395,0.58917227823316));
#7196=CARTESIAN_POINT('Ctrl Pts',(0.968701515358272,1.40840437180142,0.585702834602721));
#7197=CARTESIAN_POINT('Ctrl Pts',(1.01933067202352,1.37220157791386,0.582233390972282));
#7198=CARTESIAN_POINT('Ctrl Pts',(1.06778924659198,1.33339573546736,0.578763947341843));
#7199=CARTESIAN_POINT('Ctrl Pts',(1.11734417834837,1.29371192529939,0.575216008842412));
#7200=CARTESIAN_POINT('Ctrl Pts',(1.16462867286814,1.25130619195914,0.57166807034298));
#7201=CARTESIAN_POINT('Ctrl Pts',(1.20934754682838,1.20648107050222,0.568120131843548));
#7202=CARTESIAN_POINT('Ctrl Pts',(1.25406642078862,1.1616559490453,0.564572193344117));
#7203=CARTESIAN_POINT('Ctrl Pts',(1.29621935059572,1.11441190134086,0.561024254844686));
#7204=CARTESIAN_POINT('Ctrl Pts',(1.33555606823082,1.06508593602199,0.557476316345254));
#7205=CARTESIAN_POINT('Ctrl Pts',(1.37409908092581,1.01675523072233,0.553999965321431));
#7206=CARTESIAN_POINT('Ctrl Pts',(1.4100922720091,0.966233086539148,0.550523614297609));
#7207=CARTESIAN_POINT('Ctrl Pts',(1.44327838089219,0.91381922596826,0.547047263273786));
#7208=CARTESIAN_POINT('Ctrl Pts',(1.4766724500553,0.861076914684464,0.543549127745642));
#7209=CARTESIAN_POINT('Ctrl Pts',(1.50722375201572,0.806419454082804,0.540050992217498));
#7210=CARTESIAN_POINT('Ctrl Pts',(1.53471117517402,0.750186424361296,0.536552856689354));
#7211=CARTESIAN_POINT('Ctrl Pts',(1.56195415333876,0.694453473621678,0.533085829996392));
#7212=CARTESIAN_POINT('Ctrl Pts',(1.58618728991764,0.637173322256977,0.529618803303431));
#7213=CARTESIAN_POINT('Ctrl Pts',(1.60723987019004,0.578703777568036,0.52615177661047));
#7214=CARTESIAN_POINT('Ctrl Pts',(1.62827992233335,0.520269027379043,0.522686813102039));
#7215=CARTESIAN_POINT('Ctrl Pts',(1.6461430000243,0.460646764116287,0.519221849593608));
#7216=CARTESIAN_POINT('Ctrl Pts',(1.66070659833316,0.400214513420863,0.515756886085177));
#7217=CARTESIAN_POINT('Ctrl Pts',(1.6752668424373,0.339796181136028,0.512292720607337));
#7218=CARTESIAN_POINT('Ctrl Pts',(1.68652899719077,0.278568725063664,0.508828555129497));
#7219=CARTESIAN_POINT('Ctrl Pts',(1.69442103772059,0.216922588565335,0.505364389651658));
#7220=CARTESIAN_POINT('Ctrl Pts',(1.70244642726282,0.154234839141967,0.501841691397214));
#7221=CARTESIAN_POINT('Ctrl Pts',(1.70698664584483,0.0911146596408995,0.49831899314277));
#7222=CARTESIAN_POINT('Ctrl Pts',(1.70802086016062,0.0279786303485646,0.494796294888326));
#7223=CARTESIAN_POINT('Ctrl Pts',(1.70903916534196,-0.0341861886603169,
0.491327785673144));
#7224=CARTESIAN_POINT('Ctrl Pts',(1.70665866753178,-0.0963658581007371,
0.487859276457963));
#7225=CARTESIAN_POINT('Ctrl Pts',(1.70091210258035,-0.158164729935928,0.484390767242781));
#7226=CARTESIAN_POINT('Ctrl Pts',(1.69503086846078,-0.221411841324995,0.480840974468706));
#7227=CARTESIAN_POINT('Ctrl Pts',(1.68562385964258,-0.28425952079805,0.47729118169463));
#7228=CARTESIAN_POINT('Ctrl Pts',(1.67278165693898,-0.346294081249582,0.473741388920555));
#7229=CARTESIAN_POINT('Ctrl Pts',(1.65993945423537,-0.408328641701114,0.470191596146479));
#7230=CARTESIAN_POINT('Ctrl Pts',(1.64366226665055,-0.469549556576522,0.466641803372404));
#7231=CARTESIAN_POINT('Ctrl Pts',(1.6240943292254,-0.529561773807261,0.463092010598329));
#7232=CARTESIAN_POINT('Ctrl Pts',(1.60492317546848,-0.588357109198412,0.459614197807003));
#7233=CARTESIAN_POINT('Ctrl Pts',(1.58251700648443,-0.646227082357713,0.456136385015678));
#7234=CARTESIAN_POINT('Ctrl Pts',(1.55698484003375,-0.702791768879724,0.452658572224353));
#7235=CARTESIAN_POINT('Ctrl Pts',(1.53130481679242,-0.759684021534016,0.449160619417147));
#7236=CARTESIAN_POINT('Ctrl Pts',(1.5024625657549,-0.815255307085509,0.44566266660994));
#7237=CARTESIAN_POINT('Ctrl Pts',(1.47062003184681,-0.869134503072382,0.442164713802734));
#7238=CARTESIAN_POINT('Ctrl Pts',(1.43904583950905,-0.922559651397707,0.43869623874224));
#7239=CARTESIAN_POINT('Ctrl Pts',(1.40452198945138,-0.974320670287452,0.435227763681744));
#7240=CARTESIAN_POINT('Ctrl Pts',(1.36725357699574,-1.02407798467322,0.43175928862125));
#7241=CARTESIAN_POINT('Ctrl Pts',(1.33000743034862,-1.07380557182453,0.428292885782148));
#7242=CARTESIAN_POINT('Ctrl Pts',(1.29002027657257,-1.12153142346553,0.424826482943047));
#7243=CARTESIAN_POINT('Ctrl Pts',(1.24754019314874,-1.16694538388838,0.421360080103945));
#7244=CARTESIAN_POINT('Ctrl Pts',(1.20507002871248,-1.21234874027112,0.417894486660774));
#7245=CARTESIAN_POINT('Ctrl Pts',(1.16010843671315,-1.25544090714597,0.414428893217603));
#7246=CARTESIAN_POINT('Ctrl Pts',(1.11294204987345,-1.29594677981909,0.410963299774432));
#7247=CARTESIAN_POINT('Ctrl Pts',(1.06501750801737,-1.33710374604883,0.407442000197513));
#7248=CARTESIAN_POINT('Ctrl Pts',(1.01481704383944,-1.37559015414555,0.403920700620595));
#7249=CARTESIAN_POINT('Ctrl Pts',(0.962676466098439,-1.4111598364892,0.400399401043676));
#7250=CARTESIAN_POINT('Ctrl Pts',(0.911297074618249,-1.44621024661389,0.396929507971523));
#7251=CARTESIAN_POINT('Ctrl Pts',(0.858034319747585,-1.47842831995168,0.393459614899369));
#7252=CARTESIAN_POINT('Ctrl Pts',(0.803236798652172,-1.50762352986116,0.389989721827216));
#7253=CARTESIAN_POINT('Ctrl Pts',(0.747221538722687,-1.53746753081382,0.386442718997914));
#7254=CARTESIAN_POINT('Ctrl Pts',(0.689602974465432,-1.56415244023765,0.382895716168612));
#7255=CARTESIAN_POINT('Ctrl Pts',(0.630775216567448,-1.58752659463213,0.37934871333931));
#7256=CARTESIAN_POINT('Ctrl Pts',(0.571947458669463,-1.61090074902661,0.375801710510008));
#7257=CARTESIAN_POINT('Ctrl Pts',(0.511911057953301,-1.63096403346254,0.372254707680706));
#7258=CARTESIAN_POINT('Ctrl Pts',(0.451074060683048,-1.64761957207327,0.368707704851404));
#7259=CARTESIAN_POINT('Ctrl Pts',(0.39141703555149,-1.66395206595139,0.365229498391125));
#7260=CARTESIAN_POINT('Ctrl Pts',(0.330753587029018,-1.67707267458142,0.361751291930846));
#7261=CARTESIAN_POINT('Ctrl Pts',(0.269461118854683,-1.68686358900937,0.358273085470567));
#7262=CARTESIAN_POINT('Ctrl Pts',(0.207821550461703,-1.6967099495409,0.35477518187198));
#7263=CARTESIAN_POINT('Ctrl Pts',(0.145546295250199,-1.70318857969946,0.351277278273392));
#7264=CARTESIAN_POINT('Ctrl Pts',(0.0830343380000198,-1.70623074676695,
0.347779374674805));
#7265=CARTESIAN_POINT('Ctrl Pts',(0.0210405334683055,-1.7092476977445,0.34431046470141));
#7266=CARTESIAN_POINT('Ctrl Pts',(-0.0411855506182593,-1.70888490210486,
0.340841554728015));
#7267=CARTESIAN_POINT('Ctrl Pts',(-0.103247405107285,-1.70512698525318,
0.337372644754621));
#7268=CARTESIAN_POINT('Ctrl Pts',(-0.16527243721957,-1.70137129803887,0.333905792945793));
#7269=CARTESIAN_POINT('Ctrl Pts',(-0.227132927953601,-1.69422451512892,
0.330438941136966));
#7270=CARTESIAN_POINT('Ctrl Pts',(-0.288433314930252,-1.68372333990426,
0.326972089328139));
#7271=CARTESIAN_POINT('Ctrl Pts',(-0.349719623106744,-1.67322457647428,
0.32350603374779));
#7272=CARTESIAN_POINT('Ctrl Pts',(-0.410445583517242,-1.65937303606351,
0.320039978167441));
#7273=CARTESIAN_POINT('Ctrl Pts',(-0.470223716325484,-1.64225689802328,
0.316573922587091));
#7274=CARTESIAN_POINT('Ctrl Pts',(-0.530947338740359,-1.62487004007491,
0.313053045630207));
#7275=CARTESIAN_POINT('Ctrl Pts',(-0.59069236084168,-1.60411452105231,0.309532168673322));
#7276=CARTESIAN_POINT('Ctrl Pts',(-0.649068730272986,-1.58013538846575,
0.306011291716437));
#7277=CARTESIAN_POINT('Ctrl Pts',(-0.706607885549984,-1.55650015649181,
0.302540909986519));
#7278=CARTESIAN_POINT('Ctrl Pts',(-0.76281695348608,-1.52973345901734,0.2990705282566));
#7279=CARTESIAN_POINT('Ctrl Pts',(-0.817345024185866,-1.50002172448888,
0.295600146526682));
#7280=CARTESIAN_POINT('Ctrl Pts',(-0.873063197669847,-1.46966151629298,
0.292054021956314));
#7281=CARTESIAN_POINT('Ctrl Pts',(-0.927025640249061,-1.43622646714311,
0.288507897385946));
#7282=CARTESIAN_POINT('Ctrl Pts',(-0.978889264302855,-1.39996209617711,
0.284961772815579));
#7283=CARTESIAN_POINT('Ctrl Pts',(-1.03075288835665,-1.36369772521112,0.281415648245212));
#7284=CARTESIAN_POINT('Ctrl Pts',(-1.08051729591951,-1.32460442841043,0.277869523674845));
#7285=CARTESIAN_POINT('Ctrl Pts',(-1.12787743525702,-1.28296942813851,0.274323399104477));
#7286=CARTESIAN_POINT('Ctrl Pts',(-1.17357665734752,-1.24279456482983,0.270901636910178));
#7287=CARTESIAN_POINT('Ctrl Pts',(-1.21723191867275,-1.20008209836666,0.267479874715879));
#7288=CARTESIAN_POINT('Ctrl Pts',(-1.25854224632262,-1.15507119984926,0.26405811252158));
#7289=CARTESIAN_POINT('Ctrl Pts',(-1.29979693760062,-1.11012092159877,0.260640958725344));
#7290=CARTESIAN_POINT('Ctrl Pts',(-1.33871259591333,-1.06287872191206,0.257223804929107));
#7291=CARTESIAN_POINT('Ctrl Pts',(-1.37502237771953,-1.01362296899318,0.253806651132871));
#7292=CARTESIAN_POINT('Ctrl Pts',(-1.41129748651945,-0.964414251472054,
0.250392760451671));
#7293=CARTESIAN_POINT('Ctrl Pts',(-1.44497133744224,-0.913196209067784,
0.246978869770472));
#7294=CARTESIAN_POINT('Ctrl Pts',(-1.47581648429232,-0.860281214017284,
0.243564979089273));
#7295=CARTESIAN_POINT('Ctrl Pts',(-1.5066442567653,-0.807396024792727,0.24015301137587));
#7296=CARTESIAN_POINT('Ctrl Pts',(-1.53464621965069,-0.752816229991685,
0.236741043662468));
#7297=CARTESIAN_POINT('Ctrl Pts',(-1.55963878132793,-0.696882295856296,
0.233329075949065));
#7298=CARTESIAN_POINT('Ctrl Pts',(-1.58464105438738,-0.640926627421706,
0.229915782444293));
#7299=CARTESIAN_POINT('Ctrl Pts',(-1.60663136275903,-0.583616242298273,
0.22650248893952));
#7300=CARTESIAN_POINT('Ctrl Pts',(-1.62547330244632,-0.525313816241554,
0.223089195434747));
#7301=CARTESIAN_POINT('Ctrl Pts',(-1.64431781150788,-0.467003439795662,
0.219675436477445));
#7302=CARTESIAN_POINT('Ctrl Pts',(-1.66001295147116,-0.407701258110916,
0.216261677520142));
#7303=CARTESIAN_POINT('Ctrl Pts',(-1.67247241601735,-0.347784531227456,
0.21284791856284));
#7304=CARTESIAN_POINT('Ctrl Pts',(-1.68495043832639,-0.287778561310758,
0.20942907497859));
#7305=CARTESIAN_POINT('Ctrl Pts',(-1.69418307027723,-0.227156736665851,
0.206010231394339));
#7306=CARTESIAN_POINT('Ctrl Pts',(-1.7001355219736,-0.166304748650061,0.202591387810089));
#7307=CARTESIAN_POINT('Ctrl Pts',(-1.70559156909977,-0.11052751075362,0.199457658606699));
#7308=CARTESIAN_POINT('Ctrl Pts',(-1.7082923284714,-0.0545572754673946,
0.196323929403309));
#7309=CARTESIAN_POINT('Ctrl Pts',(-1.70824949798349,0.00130963321928915,
0.193190200199919));
#7310=CARTESIAN_POINT('Origin',(0.,0.,-1.10921167016993));
#7311=CARTESIAN_POINT('',(-0.547737204315715,1.25137522550529,6.88122480138927));
#7312=CARTESIAN_POINT('Ctrl Pts',(-0.547737204315715,1.25137522550529,6.88122480138927));
#7313=CARTESIAN_POINT('Ctrl Pts',(-0.444055474973596,1.29675756919484,6.87281718727783));
#7314=CARTESIAN_POINT('Ctrl Pts',(-0.335108563083047,1.32909106151286,6.86411225202577));
#7315=CARTESIAN_POINT('Ctrl Pts',(-0.181200932842352,1.35460353714937,6.85259070631041));
#7316=CARTESIAN_POINT('Ctrl Pts',(-0.138706804541676,1.35961230506898,6.8494816326893));
#7317=CARTESIAN_POINT('Ctrl Pts',(-0.0793406683804811,1.36379669669384,
6.84523694577867));
#7318=CARTESIAN_POINT('Ctrl Pts',(-0.0626169567451756,1.36466682082695,
6.84405188852941));
#7319=CARTESIAN_POINT('Ctrl Pts',(-0.0335989507531258,1.36564201927298,
6.84201309110666));
#7320=CARTESIAN_POINT('Ctrl Pts',(-0.021311752806731,1.36588902936461,6.84115520326926));
#7321=CARTESIAN_POINT('Ctrl Pts',(0.00412667620511559,1.3660570558976,6.83938955340606));
#7322=CARTESIAN_POINT('Ctrl Pts',(0.0172768296389448,1.36595404051807,6.83848259871138));
#7323=CARTESIAN_POINT('Ctrl Pts',(0.0517693845442809,1.36518562446532,6.83611738802191));
#7324=CARTESIAN_POINT('Ctrl Pts',(0.0731017158663196,1.36420968961024,6.8346684173855));
#7325=CARTESIAN_POINT('Ctrl Pts',(0.190616964260844,1.35606882325948,6.8267458012817));
#7326=CARTESIAN_POINT('Ctrl Pts',(0.285855327828977,1.3392334421401,6.82056909451464));
#7327=CARTESIAN_POINT('Ctrl Pts',(0.4220909484288,1.29994245299497,6.81139842562418));
#7328=CARTESIAN_POINT('Ctrl Pts',(0.464994375680968,1.28522016509727,6.8084541018543));
#7329=CARTESIAN_POINT('Ctrl Pts',(0.531466214665467,1.2586457766578,6.80369400648833));
#7330=CARTESIAN_POINT('Ctrl Pts',(0.555560869782164,1.24819767870632,6.80192541601101));
#7331=CARTESIAN_POINT('Ctrl Pts',(0.588279607063654,1.23287493246639,6.79944399880338));
#7332=CARTESIAN_POINT('Ctrl Pts',(0.597175573755726,1.22859058079316,6.7987610043893));
#7333=CARTESIAN_POINT('Ctrl Pts',(0.612271321412319,1.22111769395799,6.79758643684037));
#7334=CARTESIAN_POINT('Ctrl Pts',(0.618494767536184,1.21797734531252,6.79709761695324));
#7335=CARTESIAN_POINT('Ctrl Pts',(0.631763955612415,1.21115379244051,6.79604501855935));
#7336=CARTESIAN_POINT('Ctrl Pts',(0.638801942834561,1.20745653106315,6.79548046141145));
#7337=CARTESIAN_POINT('Ctrl Pts',(0.659131988689208,1.19654907358243,6.79383226734929));
#7338=CARTESIAN_POINT('Ctrl Pts',(0.672336639391703,1.18917957435487,6.79273994674508));
#7339=CARTESIAN_POINT('Ctrl Pts',(0.746188488001,1.14633976986416,6.78651741449112));
#7340=CARTESIAN_POINT('Ctrl Pts',(0.804146072057655,1.10645361193097,6.78120229325178));
#7341=CARTESIAN_POINT('Ctrl Pts',(0.908653805019832,1.02196783577947,6.77104647106142));
#7342=CARTESIAN_POINT('Ctrl Pts',(0.955635717510016,0.978177759687796,6.76621672168241));
#7343=CARTESIAN_POINT('Ctrl Pts',(1.02616944010302,0.902484174838384,6.75860017586617));
#7344=CARTESIAN_POINT('Ctrl Pts',(1.0517174803317,0.872577950102533,6.75574862906286));
#7345=CARTESIAN_POINT('Ctrl Pts',(1.08589247066364,0.828887433979547,6.75179622020007));
#7346=CARTESIAN_POINT('Ctrl Pts',(1.09561690389833,0.815990487313167,6.75065405063617));
#7347=CARTESIAN_POINT('Ctrl Pts',(1.11220629378608,0.793157540214015,6.74867333090079));
#7348=CARTESIAN_POINT('Ctrl Pts',(1.11917230506538,0.783297575307153,6.747831050253));
#7349=CARTESIAN_POINT('Ctrl Pts',(1.13342987687498,0.762538279518553,6.74608401406562));
#7350=CARTESIAN_POINT('Ctrl Pts',(1.14069707302286,0.751623656841593,6.7451802174939));
#7351=CARTESIAN_POINT('Ctrl Pts',(1.15957263621349,0.722369916348837,6.74279520509396));
#7352=CARTESIAN_POINT('Ctrl Pts',(1.17090330182126,0.703855481007286,6.74132399678973));
#7353=CARTESIAN_POINT('Ctrl Pts',(1.23174853529083,0.598894886043928,6.73317681849201));
#7354=CARTESIAN_POINT('Ctrl Pts',(1.27213241774242,0.507504613871995,6.72682833630085));
#7355=CARTESIAN_POINT('Ctrl Pts',(1.31650773539199,0.36742581360311,6.71737009128827));
#7356=CARTESIAN_POINT('Ctrl Pts',(1.32844184238847,0.321614716899254,6.71431170350496));
#7357=CARTESIAN_POINT('Ctrl Pts',(1.34171051078477,0.257123565763821,6.70994545798023));
#7358=CARTESIAN_POINT('Ctrl Pts',(1.34507599310962,0.238893546980178,6.70870449104615));
#7359=CARTESIAN_POINT('Ctrl Pts',(1.35035718418356,0.206620841289652,6.70648689448736));
#7360=CARTESIAN_POINT('Ctrl Pts',(1.3524272967231,0.19260598292506,6.70551703664031));
#7361=CARTESIAN_POINT('Ctrl Pts',(1.35528668381136,0.170919373947805,6.70400223335901));
#7362=CARTESIAN_POINT('Ctrl Pts',(1.35622964181346,0.16326842634506,6.70346512861712));
#7363=CARTESIAN_POINT('Ctrl Pts',(1.35788104280237,0.148866222001141,6.70244833728836));
#7364=CARTESIAN_POINT('Ctrl Pts',(1.358603993953,0.142117056891211,6.70196942000449));
#7365=CARTESIAN_POINT('Ctrl Pts',(1.36023955539263,0.125693210825868,6.70079834020808));
#7366=CARTESIAN_POINT('Ctrl Pts',(1.36109926562933,0.116013819553316,6.70010345493855));
#7367=CARTESIAN_POINT('Ctrl Pts',(1.36378012987047,0.0816766431119194,6.69762359453806));
#7368=CARTESIAN_POINT('Ctrl Pts',(1.3650349135384,0.0569808877648533,6.69581311537244));
#7369=CARTESIAN_POINT('Ctrl Pts',(1.36747715358494,-0.046381986422803,6.68815751231844));
#7370=CARTESIAN_POINT('Ctrl Pts',(1.36253775704882,-0.125041302655787,6.6821529400915));
#7371=CARTESIAN_POINT('Ctrl Pts',(1.33978057399129,-0.276600634351956,6.67060515621317));
#7372=CARTESIAN_POINT('Ctrl Pts',(1.3226798455,-0.349343878997171,6.66507322849514));
#7373=CARTESIAN_POINT('Ctrl Pts',(1.29387729252783,-0.438404063292854,6.65836244419621));
#7374=CARTESIAN_POINT('Ctrl Pts',(1.28765787036867,-0.456348380546274,6.65701294683789));
#7375=CARTESIAN_POINT('Ctrl Pts',(1.27673948944134,-0.485847337380051,6.65479769760526));
#7376=CARTESIAN_POINT('Ctrl Pts',(1.27225303688697,-0.497477223193274,6.65392517179943));
#7377=CARTESIAN_POINT('Ctrl Pts',(1.26312380975889,-0.520210564038238,6.65222061199698));
#7378=CARTESIAN_POINT('Ctrl Pts',(1.25849225947018,-0.531317267461592,6.6513882990959));
#7379=CARTESIAN_POINT('Ctrl Pts',(1.24792131460961,-0.555752893250382,6.6495573522297));
#7380=CARTESIAN_POINT('Ctrl Pts',(1.24191384743358,-0.569050884201948,6.64856108504092));
#7381=CARTESIAN_POINT('Ctrl Pts',(1.21965528737674,-0.616289615053219,6.64501948766852));
#7382=CARTESIAN_POINT('Ctrl Pts',(1.20221571569978,-0.649653501749628,6.64251392485358));
#7383=CARTESIAN_POINT('Ctrl Pts',(1.11883228547365,-0.79428748449609,6.63154375565138));
#7384=CARTESIAN_POINT('Ctrl Pts',(1.03867526544744,-0.896562574527913,6.6235514454688));
#7385=CARTESIAN_POINT('Ctrl Pts',(0.930589519284609,-1.00018866743715,6.6135292465496));
#7386=CARTESIAN_POINT('Ctrl Pts',(0.915512462838768,-1.01400741890669,6.6121437847811));
#7387=CARTESIAN_POINT('Ctrl Pts',(0.893495140935552,-1.03329583617809,6.61012830546018));
#7388=CARTESIAN_POINT('Ctrl Pts',(0.886802401097707,-1.03904539970548,6.60951663296651));
#7389=CARTESIAN_POINT('Ctrl Pts',(0.875427741473142,-1.04862713546565,6.60847777138842));
#7390=CARTESIAN_POINT('Ctrl Pts',(0.870775270048772,-1.05249371780724,6.60805301974325));
#7391=CARTESIAN_POINT('Ctrl Pts',(0.859958841950382,-1.06136223733428,6.60706575744925));
#7392=CARTESIAN_POINT('Ctrl Pts',(0.853776972137215,-1.06634135366425,6.60650176016272));
#7393=CARTESIAN_POINT('Ctrl Pts',(0.835904612804853,-1.0804814051409,6.60487273376766));
#7394=CARTESIAN_POINT('Ctrl Pts',(0.824108033693321,-1.08950561822569,6.60379937489742));
#7395=CARTESIAN_POINT('Ctrl Pts',(0.764459048151997,-1.13361324016885,6.59839038343062));
#7396=CARTESIAN_POINT('Ctrl Pts',(0.71450708418842,-1.16574224508069,6.59392164862438));
#7397=CARTESIAN_POINT('Ctrl Pts',(0.599224813697061,-1.22969222547908,6.58395374840633));
#7398=CARTESIAN_POINT('Ctrl Pts',(0.533114025374813,-1.25976367082325,6.57846521073137));
#7399=CARTESIAN_POINT('Ctrl Pts',(0.425337394258642,-1.29877501379294,6.57000324915296));
#7400=CARTESIAN_POINT('Ctrl Pts',(0.385106074064548,-1.31126747803365,6.56694293905821));
#7401=CARTESIAN_POINT('Ctrl Pts',(0.328382092306131,-1.32604440020571,6.56276279052938));
#7402=CARTESIAN_POINT('Ctrl Pts',(0.312331474880023,-1.32991640411673,6.56159452039775));
#7403=CARTESIAN_POINT('Ctrl Pts',(0.284394900029043,-1.33612204680169,6.55958523991947));
#7404=CARTESIAN_POINT('Ctrl Pts',(0.272541129647848,-1.3385902779876,6.55874012991516));
#7405=CARTESIAN_POINT('Ctrl Pts',(0.247959032714924,-1.3433687567822,6.55700224499999));
#7406=CARTESIAN_POINT('Ctrl Pts',(0.235227525636655,-1.34565646782956,6.55611024625341));
#7407=CARTESIAN_POINT('Ctrl Pts',(0.201835883054979,-1.35116817387901,6.55379051031716));
#7408=CARTESIAN_POINT('Ctrl Pts',(0.181130397009088,-1.35409933680979,6.55237181185296));
#7409=CARTESIAN_POINT('Ctrl Pts',(0.0573245200133942,-1.36873502905124,
6.54398948635327));
#7410=CARTESIAN_POINT('Ctrl Pts',(-0.0467682713600107,-1.36913718191617,
6.53738834890233));
#7411=CARTESIAN_POINT('Ctrl Pts',(-0.193737416610724,-1.35291022430366,
6.52785222370281));
#7412=CARTESIAN_POINT('Ctrl Pts',(-0.237302096321603,-1.34595225351311,
6.52499278431376));
#7413=CARTESIAN_POINT('Ctrl Pts',(-0.305717043762331,-1.33160037489074,
6.52034896384995));
#7414=CARTESIAN_POINT('Ctrl Pts',(-0.3308259542693,-1.32558532599812,6.51861100259614));
#7415=CARTESIAN_POINT('Ctrl Pts',(-0.365093904570292,-1.31634195917769,
6.51617372705014));
#7416=CARTESIAN_POINT('Ctrl Pts',(-0.374412981246757,-1.31372166704474,
6.51550417736877));
#7417=CARTESIAN_POINT('Ctrl Pts',(-0.390252564147855,-1.30908575212468,
6.51435337834624));
#7418=CARTESIAN_POINT('Ctrl Pts',(-0.396787196556692,-1.3071199213282,6.51387486167448));
#7419=CARTESIAN_POINT('Ctrl Pts',(-0.410761282430147,-1.30280161206176,
6.51284309939162));
#7420=CARTESIAN_POINT('Ctrl Pts',(-0.41819539404998,-1.30043434140424,6.51228911234275));
#7421=CARTESIAN_POINT('Ctrl Pts',(-0.43909712741647,-1.29358077245566,6.51071789339233));
#7422=CARTESIAN_POINT('Ctrl Pts',(-0.452515254216709,-1.28894817855045,
6.50969318499319));
#7423=CARTESIAN_POINT('Ctrl Pts',(-0.558815381398263,-1.25038382966089,
6.50145965743748));
#7424=CARTESIAN_POINT('Ctrl Pts',(-0.647830599009339,-1.20666826675332,
6.49388108254749));
#7425=CARTESIAN_POINT('Ctrl Pts',(-0.786348944914703,-1.11886225427749,
6.48154920476506));
#7426=CARTESIAN_POINT('Ctrl Pts',(-0.838796995776625,-1.08010143497704,
6.47672399020658));
#7427=CARTESIAN_POINT('Ctrl Pts',(-0.904636482967574,-1.02374415881705,
6.47048323590923));
#7428=CARTESIAN_POINT('Ctrl Pts',(-0.920655554718127,-1.00936252734762,
6.46894826253573));
#7429=CARTESIAN_POINT('Ctrl Pts',(-0.945821840723968,-0.985670851127824,
6.46650821723242));
#7430=CARTESIAN_POINT('Ctrl Pts',(-0.955186645712328,-0.976598419951707,
6.46559354564364));
#7431=CARTESIAN_POINT('Ctrl Pts',(-0.972935791576037,-0.958903813543366,
6.46384624658676));
#7432=CARTESIAN_POINT('Ctrl Pts',(-0.981338931448249,-0.95030231812153,
6.4630128496364));
#7433=CARTESIAN_POINT('Ctrl Pts',(-1.00054117584257,-0.93012043771098,6.4610931195179));
#7434=CARTESIAN_POINT('Ctrl Pts',(-1.0112548276038,-0.918460876587213,6.46001042243936));
#7435=CARTESIAN_POINT('Ctrl Pts',(-1.04531087051077,-0.880079488115456,
6.45652700759092));
#7436=CARTESIAN_POINT('Ctrl Pts',(-1.06781655698413,-0.852632893999194,
6.4541594263214));
#7437=CARTESIAN_POINT('Ctrl Pts',(-1.16850257324679,-0.71959277086434,6.44316659660916));
#7438=CARTESIAN_POINT('Ctrl Pts',(-1.23224079855161,-0.603976015019015,
6.43504592501645));
#7439=CARTESIAN_POINT('Ctrl Pts',(-1.28575916397003,-0.46174153678167,6.42487262525093));
#7440=CARTESIAN_POINT('Ctrl Pts',(-1.29258758701473,-0.442265863486875,
6.42347441551532));
#7441=CARTESIAN_POINT('Ctrl Pts',(-1.30172338697076,-0.414187532268361,
6.42144113458031));
#7442=CARTESIAN_POINT('Ctrl Pts',(-1.30439220737305,-0.40570438321826,6.42082457909091));
#7443=CARTESIAN_POINT('Ctrl Pts',(-1.30874482811647,-0.391382038252033,
6.41977889754312));
#7444=CARTESIAN_POINT('Ctrl Pts',(-1.31047281802553,-0.385556631417649,
6.41935224775471));
#7445=CARTESIAN_POINT('Ctrl Pts',(-1.31436706645888,-0.372099640699887,
6.41836338156362));
#7446=CARTESIAN_POINT('Ctrl Pts',(-1.31650570863623,-0.364460751156839,
6.4177997065548));
#7447=CARTESIAN_POINT('Ctrl Pts',(-1.3224595694033,-0.342458112451721,6.41617024721395));
#7448=CARTESIAN_POINT('Ctrl Pts',(-1.32610693607016,-0.328050636719565,
6.41509610514067));
#7449=CARTESIAN_POINT('Ctrl Pts',(-1.34502775195454,-0.247831913845801,
6.40908613189534));
#7450=CARTESIAN_POINT('Ctrl Pts',(-1.35563628089949,-0.181022156970859,
6.40397686935053));
#7451=CARTESIAN_POINT('Ctrl Pts',(-1.36873956463937,-0.0241564204154046,
6.39206829691884));
#7452=CARTESIAN_POINT('Ctrl Pts',(-1.36736595253409,0.0659287662872278,
6.38530757367569));
#7453=CARTESIAN_POINT('Ctrl Pts',(-1.35435234407392,0.179699755680297,6.37702130393148));
#7454=CARTESIAN_POINT('Ctrl Pts',(-1.35089308083831,0.204084043171095,6.37525875774045));
#7455=CARTESIAN_POINT('Ctrl Pts',(-1.34449507938174,0.241816421596295,6.37255067299858));
#7456=CARTESIAN_POINT('Ctrl Pts',(-1.34201234030731,0.255235386774298,6.37159138250401));
#7457=CARTESIAN_POINT('Ctrl Pts',(-1.33699345692545,0.280259778058949,6.36980885250657));
#7458=CARTESIAN_POINT('Ctrl Pts',(-1.33450623065413,0.291873573576734,6.36898418130947));
#7459=CARTESIAN_POINT('Ctrl Pts',(-1.32855036073377,0.318014066022518,6.36713310918047));
#7460=CARTESIAN_POINT('Ctrl Pts',(-1.3249942881647,0.332519432817389,6.36610954342743));
#7461=CARTESIAN_POINT('Ctrl Pts',(-1.31315609531256,0.377597967257694,6.36293715588306));
#7462=CARTESIAN_POINT('Ctrl Pts',(-1.30404781334725,0.407944483190907,6.36081417736566));
#7463=CARTESIAN_POINT('Ctrl Pts',(-1.25775384022177,0.54471708888294,6.35125293892159));
#7464=CARTESIAN_POINT('Ctrl Pts',(-1.20854286930759,0.646594109476209,6.34418992000542));
#7465=CARTESIAN_POINT('Ctrl Pts',(-1.14737960347042,0.741266514514222,6.33682691740051));
#7466=CARTESIAN_POINT('',(0.995642551412613,0.935228266155693,6.88122480138927));
#7467=CARTESIAN_POINT('Origin',(0.,0.,6.88122480138927));
#7468=CARTESIAN_POINT('',(-1.36599994346263,0.000393014108642856,6.50921167020825));
#7469=CARTESIAN_POINT('Ctrl Pts',(-1.36599994346263,0.000393014108642897,
6.50921167020824));
#7470=CARTESIAN_POINT('Ctrl Pts',(-1.36601509581434,-0.0522720457987859,
6.51291417912242));
#7471=CARTESIAN_POINT('Ctrl Pts',(-1.36298002712899,-0.105055605456886,
6.5166166880366));
#7472=CARTESIAN_POINT('Ctrl Pts',(-1.35688129899332,-0.15757265131422,6.52031919695078));
#7473=CARTESIAN_POINT('Ctrl Pts',(-1.35087780158986,-0.209269651316286,
6.52396389173928));
#7474=CARTESIAN_POINT('Ctrl Pts',(-1.34190568289767,-0.260707838473859,
6.52760858652779));
#7475=CARTESIAN_POINT('Ctrl Pts',(-1.33000442155041,-0.311519242834772,
6.53125328131629));
#7476=CARTESIAN_POINT('Ctrl Pts',(-1.31811417516861,-0.362283619754845,
6.53489460283317));
#7477=CARTESIAN_POINT('Ctrl Pts',(-1.30330027692159,-0.412421833881958,
6.53853592435005));
#7478=CARTESIAN_POINT('Ctrl Pts',(-1.28565356051786,-0.461574395225452,
6.54217724586693));
#7479=CARTESIAN_POINT('Ctrl Pts',(-1.26801571849919,-0.51070223815982,6.54581673619389));
#7480=CARTESIAN_POINT('Ctrl Pts',(-1.24754806506583,-0.558844898258482,
6.54945622652084));
#7481=CARTESIAN_POINT('Ctrl Pts',(-1.22439101530232,-0.605658849226993,
6.5530957168478));
#7482=CARTESIAN_POINT('Ctrl Pts',(-1.20054346040706,-0.653868715206742,
6.55684373078952));
#7483=CARTESIAN_POINT('Ctrl Pts',(-1.17384374886831,-0.700668785653974,
6.56059174473125));
#7484=CARTESIAN_POINT('Ctrl Pts',(-1.14449700594271,-0.745709463120968,
6.56433975867297));
#7485=CARTESIAN_POINT('Ctrl Pts',(-1.11597450395673,-0.789485115354654,
6.56798250483282));
#7486=CARTESIAN_POINT('Ctrl Pts',(-1.08495211768822,-0.831598503119688,
6.57162525099267));
#7487=CARTESIAN_POINT('Ctrl Pts',(-1.05166136614232,-0.871759353814842,
6.57526799715252));
#7488=CARTESIAN_POINT('Ctrl Pts',(-1.01692756445579,-0.913661051999237,
6.57906864498518));
#7489=CARTESIAN_POINT('Ctrl Pts',(-0.979724640210714,-0.953436539582381,
6.58286929281784));
#7490=CARTESIAN_POINT('Ctrl Pts',(-0.940358579361482,-0.990798537655993,
6.5866699406505));
#7491=CARTESIAN_POINT('Ctrl Pts',(-0.900992518512251,-1.02816053572961,
6.59047058848316));
#7492=CARTESIAN_POINT('Ctrl Pts',(-0.859463877262655,-1.06310867126732,
6.59427123631583));
#7493=CARTESIAN_POINT('Ctrl Pts',(-0.816114854989169,-1.09540519601927,
6.59807188414849));
#7494=CARTESIAN_POINT('Ctrl Pts',(-0.774111632074759,-1.12669905358215,
6.60175453832988));
#7495=CARTESIAN_POINT('Ctrl Pts',(-0.730220153355013,-1.15563740902186,
6.60543719251126));
#7496=CARTESIAN_POINT('Ctrl Pts',(-0.684734362040178,-1.1819876705962,6.60911984669265));
#7497=CARTESIAN_POINT('Ctrl Pts',(-0.639327745912801,-1.20829206538798,
6.61279609063412));
#7498=CARTESIAN_POINT('Ctrl Pts',(-0.592332782989818,-1.23201703962708,
6.61647233457559));
#7499=CARTESIAN_POINT('Ctrl Pts',(-0.544073299409954,-1.25297256349418,
6.62014857851706));
#7500=CARTESIAN_POINT('Ctrl Pts',(-0.495860259417331,-1.27390792034686,
6.62382128454342));
#7501=CARTESIAN_POINT('Ctrl Pts',(-0.446385597455214,-1.2920788943395,6.62749399056977));
#7502=CARTESIAN_POINT('Ctrl Pts',(-0.395996943868893,-1.30734173820256,
6.63116669659613));
#7503=CARTESIAN_POINT('Ctrl Pts',(-0.345636451000062,-1.32259605211685,
6.6348373500565));
#7504=CARTESIAN_POINT('Ctrl Pts',(-0.294363489648552,-1.33494530272762,
6.63850800351686));
#7505=CARTESIAN_POINT('Ctrl Pts',(-0.242542566451201,-1.34429502099028,
6.64217865697723));
#7506=CARTESIAN_POINT('Ctrl Pts',(-0.190729696309135,-1.3536432862916,6.64584874001211));
#7507=CARTESIAN_POINT('Ctrl Pts',(-0.138369559335716,-1.35999285101895,
6.64951882304699));
#7508=CARTESIAN_POINT('Ctrl Pts',(-0.0858362412672093,-1.36330045833085,
6.65318890608187));
#7509=CARTESIAN_POINT('Ctrl Pts',(-0.0332532529394221,-1.36661119298591,
6.65686245918075));
#7510=CARTESIAN_POINT('Ctrl Pts',(0.0195027089561627,-1.36687419367247,
6.66053601227963));
#7511=CARTESIAN_POINT('Ctrl Pts',(0.0720546955455641,-1.36409828122824,
6.66420956537851));
#7512=CARTESIAN_POINT('Ctrl Pts',(0.124633440876391,-1.36132095532796,6.66788498899959));
#7513=CARTESIAN_POINT('Ctrl Pts',(0.177007472065912,-1.35550169225283,6.67156041262067));
#7514=CARTESIAN_POINT('Ctrl Pts',(0.228805481142311,-1.34670117390579,6.67523583624175));
#7515=CARTESIAN_POINT('Ctrl Pts',(0.280697525684336,-1.33788467886669,6.67891793232337));
#7516=CARTESIAN_POINT('Ctrl Pts',(0.33201093872555,-1.32607624239086,6.68260002840499));
#7517=CARTESIAN_POINT('Ctrl Pts',(0.382386508246656,-1.31138726481194,6.68628212448661));
#7518=CARTESIAN_POINT('Ctrl Pts',(0.410542758955961,-1.30317720308346,6.68834014628955));
#7519=CARTESIAN_POINT('Ctrl Pts',(0.438406326130136,-1.294068154454,6.69039816809249));
#7520=CARTESIAN_POINT('Ctrl Pts',(0.465917295775467,-1.28408608492471,6.69245618989542));
#7521=CARTESIAN_POINT('Ctrl Pts',(0.514537992252857,-1.26644457031957,6.69609337370662));
#7522=CARTESIAN_POINT('Ctrl Pts',(0.562270734526597,-1.2459956382712,6.69973055751783));
#7523=CARTESIAN_POINT('Ctrl Pts',(0.608765467660196,-1.22284937968029,6.70336774132903));
#7524=CARTESIAN_POINT('Ctrl Pts',(0.655177339783475,-1.19974437140404,6.70699844310011));
#7525=CARTESIAN_POINT('Ctrl Pts',(0.700355089214269,-1.17395180847786,6.7106291448712));
#7526=CARTESIAN_POINT('Ctrl Pts',(0.743967007168403,-1.14563043440932,6.71425984664229));
#7527=CARTESIAN_POINT('Ctrl Pts',(0.787536231813736,-1.11733678517439,6.71788699418602));
#7528=CARTESIAN_POINT('Ctrl Pts',(0.829542199504999,-1.08651952047162,6.72151414172975));
#7529=CARTESIAN_POINT('Ctrl Pts',(0.869678231376943,-1.05338301385065,6.72514128927348));
#7530=CARTESIAN_POINT('Ctrl Pts',(0.909792204127563,-1.02026471934945,6.72876644330454));
#7531=CARTESIAN_POINT('Ctrl Pts',(0.948037853104004,-0.984830055780476,
6.73239159733561));
#7532=CARTESIAN_POINT('Ctrl Pts',(0.984140051541839,-0.947324843414985,
6.73601675136667));
#7533=CARTESIAN_POINT('Ctrl Pts',(1.02023790633019,-0.909824143503118,6.73964146923598));
#7534=CARTESIAN_POINT('Ctrl Pts',(1.0541924424754,-0.870253785592282,6.74326618710529));
#7535=CARTESIAN_POINT('Ctrl Pts',(1.0857658945044,-0.828895905606408,6.7468909049746));
#7536=CARTESIAN_POINT('Ctrl Pts',(1.11737436806205,-0.787492151125154,6.75051964341031));
#7537=CARTESIAN_POINT('Ctrl Pts',(1.14659615148461,-0.744297354419688,6.75414838184603));
#7538=CARTESIAN_POINT('Ctrl Pts',(1.1732353468568,-0.699624771492414,6.75777712028175));
#7539=CARTESIAN_POINT('Ctrl Pts',(1.19988999970509,-0.65492626715971,6.76140796430426));
#7540=CARTESIAN_POINT('Ctrl Pts',(1.22395883083609,-0.608748759074452,6.76503880832676));
#7541=CARTESIAN_POINT('Ctrl Pts',(1.2452924679255,-0.56142913117152,6.76866965234926));
#7542=CARTESIAN_POINT('Ctrl Pts',(1.26667062895704,-0.514010745782216,6.77230807405242));
#7543=CARTESIAN_POINT('Ctrl Pts',(1.28530200708757,-0.465445996734002,6.77594649575558));
#7544=CARTESIAN_POINT('Ctrl Pts',(1.30108634062948,-0.416089334431191,6.77958491745874));
#7545=CARTESIAN_POINT('Ctrl Pts',(1.31157847846954,-0.383281050012264,6.78200344351994));
#7546=CARTESIAN_POINT('Ctrl Pts',(1.32081369083876,-0.350123165431055,6.78442196958114));
#7547=CARTESIAN_POINT('Ctrl Pts',(1.32877511797438,-0.316721779882873,6.78684049564234));
#7548=CARTESIAN_POINT('Ctrl Pts',(1.34172091212639,-0.262408972099444,6.79077317504847));
#7549=CARTESIAN_POINT('Ctrl Pts',(1.35135491722136,-0.207204138267393,6.79470585445459));
#7550=CARTESIAN_POINT('Ctrl Pts',(1.35756883720119,-0.15153498691791,6.79863853386071));
#7551=CARTESIAN_POINT('Ctrl Pts',(1.36352526533053,-0.0981726487946194,
6.80240825125558));
#7552=CARTESIAN_POINT('Ctrl Pts',(1.36633940003821,-0.044384275270335,6.80617796865046));
#7553=CARTESIAN_POINT('Ctrl Pts',(1.36596737288208,0.00944119810278521,
6.80994768604533));
#7554=CARTESIAN_POINT('Ctrl Pts',(1.3655958134874,0.063198995016105,6.81371266365601));
#7555=CARTESIAN_POINT('Ctrl Pts',(1.36204604684839,0.116993301466068,6.81747764126669));
#7556=CARTESIAN_POINT('Ctrl Pts',(1.35532611850322,0.170432134596119,6.82124261887738));
#7557=CARTESIAN_POINT('Ctrl Pts',(1.34861248442448,0.223820913880939,6.82500406999626));
#7558=CARTESIAN_POINT('Ctrl Pts',(1.33873464674067,0.276854385991406,6.82876552111515));
#7559=CARTESIAN_POINT('Ctrl Pts',(1.32575254381536,0.329144637761449,6.83252697223403));
#7560=CARTESIAN_POINT('Ctrl Pts',(1.31277844339189,0.381402656476579,6.83628610469779));
#7561=CARTESIAN_POINT('Ctrl Pts',(1.29670399995535,0.432917880211148,6.84004523716155));
#7562=CARTESIAN_POINT('Ctrl Pts',(1.27764003146218,0.483313511093276,6.84380436962531));
#7563=CARTESIAN_POINT('Ctrl Pts',(1.25857628906331,0.533708544294783,6.84756345750662));
#7564=CARTESIAN_POINT('Ctrl Pts',(1.2365232586372,0.582983539062316,6.85132254538793));
#7565=CARTESIAN_POINT('Ctrl Pts',(1.21164079598937,0.630779344536778,6.85508163326924));
#7566=CARTESIAN_POINT('Ctrl Pts',(1.18675908331869,0.678573709407772,6.85884060784866));
#7567=CARTESIAN_POINT('Ctrl Pts',(1.15904834615365,0.724888533338292,6.86259958242808));
#7568=CARTESIAN_POINT('Ctrl Pts',(1.12871443519632,0.769389188759139,6.8663585570075));
#7569=CARTESIAN_POINT('Ctrl Pts',(1.09835975702567,0.813920310235141,6.87012010505748));
#7570=CARTESIAN_POINT('Ctrl Pts',(1.0653786097342,0.856634375336335,6.87388165310747));
#7571=CARTESIAN_POINT('Ctrl Pts',(1.03001932871992,0.897226940335258,6.87764320115746));
#7572=CARTESIAN_POINT('Ctrl Pts',(1.01879674984241,0.910110495924438,6.87883706790139));
#7573=CARTESIAN_POINT('Ctrl Pts',(1.00733490922091,0.922780600295316,6.88003093464533));
#7574=CARTESIAN_POINT('Ctrl Pts',(0.995642551412613,0.935228266155693,6.88122480138927));
#7575=CARTESIAN_POINT('Ctrl Pts',(-1.36599996455079,0.000311202912832261,
6.50809119519899));
#7576=CARTESIAN_POINT('Ctrl Pts',(-1.36599754429993,0.0109346978751973,
6.50731552338978));
#7577=CARTESIAN_POINT('Ctrl Pts',(-1.3658711942542,0.0215582237833071,6.50654460410721));
#7578=CARTESIAN_POINT('Ctrl Pts',(-1.36540521978107,0.0413330020605039,
6.50511969138689));
#7579=CARTESIAN_POINT('Ctrl Pts',(-1.36509749686988,0.0504843237358567,
6.50446429910442));
#7580=CARTESIAN_POINT('Ctrl Pts',(-1.36442613075401,0.065848712042639,6.50337144265674));
#7581=CARTESIAN_POINT('Ctrl Pts',(-1.36411201052067,0.0720634853177237,
6.50293145367623));
#7582=CARTESIAN_POINT('Ctrl Pts',(-1.36334680897726,0.0853951199963837,
6.50199233947414));
#7583=CARTESIAN_POINT('Ctrl Pts',(-1.36288244499507,0.0925110488199359,
6.50149398442202));
#7584=CARTESIAN_POINT('Ctrl Pts',(-1.36151936875785,0.111151324983536,6.50019539616074));
#7585=CARTESIAN_POINT('Ctrl Pts',(-1.36053004394861,0.122668784287314,6.49939990292469));
#7586=CARTESIAN_POINT('Ctrl Pts',(-1.35506128540604,0.178076452606176,6.49560011419122));
#7587=CARTESIAN_POINT('Ctrl Pts',(-1.34860313287363,0.221749230337503,6.49268687248508));
#7588=CARTESIAN_POINT('Ctrl Pts',(-1.32095139951885,0.361557908053979,6.48340854333537));
#7589=CARTESIAN_POINT('Ctrl Pts',(-1.29148954239672,0.455732446889767,6.4772123244871));
#7590=CARTESIAN_POINT('Ctrl Pts',(-1.23672911706547,0.581333874140369,6.46820920164614));
#7591=CARTESIAN_POINT('Ctrl Pts',(-1.21979842017135,0.616067672157524,6.46563716173223));
#7592=CARTESIAN_POINT('Ctrl Pts',(-1.19382967997553,0.664064090731224,6.46193362099985));
#7593=CARTESIAN_POINT('Ctrl Pts',(-1.18599445445098,0.677958361132938,6.46084315922013));
#7594=CARTESIAN_POINT('Ctrl Pts',(-1.17187685057423,0.701999270083489,6.45892207678362));
#7595=CARTESIAN_POINT('Ctrl Pts',(-1.16570136031198,0.71220688770795,6.45809531679904));
#7596=CARTESIAN_POINT('Ctrl Pts',(-1.1554403742083,0.728676483761021,6.45674261975205));
#7597=CARTESIAN_POINT('Ctrl Pts',(-1.15143572786607,0.734988186398318,6.45621965924215));
#7598=CARTESIAN_POINT('Ctrl Pts',(-1.14737960337948,0.741266514654979,6.45569480720057));
#7599=CARTESIAN_POINT('Ctrl Pts',(-0.595951749398983,1.22654481333082,-0.198948690821724));
#7600=CARTESIAN_POINT('Ctrl Pts',(-1.0000533487054,1.03020053595575,-0.167487255572748));
#7601=CARTESIAN_POINT('Ctrl Pts',(-1.59252126055165,0.210609571278056,-0.104564385074798));
#7602=CARTESIAN_POINT('Ctrl Pts',(-1.0508036035899,-1.21692831989964,-0.0101800793278729));
#7603=CARTESIAN_POINT('Ctrl Pts',(0.437846824792563,-1.54552130761885,0.0842042264190528));
#7604=CARTESIAN_POINT('Ctrl Pts',(1.53180658334325,-0.485155857487698,0.178588532165979));
#7605=CARTESIAN_POINT('Ctrl Pts',(1.24759243572345,1.01280491202726,0.272972837912904));
#7606=CARTESIAN_POINT('Ctrl Pts',(-0.159548416134459,1.59879372907719,0.36735714365983));
#7607=CARTESIAN_POINT('Ctrl Pts',(-1.42301181748291,0.746252543525721,0.461741449406754));
#7608=CARTESIAN_POINT('Ctrl Pts',(-1.40591424239536,-0.778006731171808,
0.556125755153681));
#7609=CARTESIAN_POINT('Ctrl Pts',(-0.123566114012858,-1.60203927132338,
0.650510060900605));
#7610=CARTESIAN_POINT('Ctrl Pts',(1.26996906566004,-0.98438823499133,0.744894366647532));
#7611=CARTESIAN_POINT('Ctrl Pts',(1.52062832125674,0.519164000491415,0.839278672394458));
#7612=CARTESIAN_POINT('Ctrl Pts',(0.402824829336517,1.55549410206089,0.933662978141383));
#7613=CARTESIAN_POINT('Ctrl Pts',(-1.0774907814505,1.19199423922429,1.02804728388831));
#7614=CARTESIAN_POINT('Ctrl Pts',(-1.58814124060392,-0.244219928936947,
1.12243158963524));
#7615=CARTESIAN_POINT('Ctrl Pts',(-0.669575311644667,-1.46065169016511,
1.21681589538216));
#7616=CARTESIAN_POINT('Ctrl Pts',(0.851561190150558,-1.36260011027521,1.31120020112909));
#7617=CARTESIAN_POINT('Ctrl Pts',(1.60635244239379,-0.0383034713654621,
1.40558450687601));
#7618=CARTESIAN_POINT('Ctrl Pts',(0.915538973494178,1.32046337807201,1.49996881262294));
#7619=CARTESIAN_POINT('Ctrl Pts',(-0.599195377524483,1.49090583294604,1.59435311836986));
#7620=CARTESIAN_POINT('Ctrl Pts',(-1.57469589658012,0.319637442586392,1.68873742411679));
#7621=CARTESIAN_POINT('Ctrl Pts',(-1.13308043611877,-1.13928221574075,1.78312172986372));
#7622=CARTESIAN_POINT('Ctrl Pts',(0.328228015712479,-1.57292772700279,1.87750603561064));
#7623=CARTESIAN_POINT('Ctrl Pts',(1.49415425557531,-0.591048489903462,1.97189034135757));
#7624=CARTESIAN_POINT('Ctrl Pts',(1.31544635921791,0.922732968463878,2.06627464710449));
#7625=CARTESIAN_POINT('Ctrl Pts',(-0.0470710861353782,1.60611941371602,
2.16065895285142));
#7626=CARTESIAN_POINT('Ctrl Pts',(-1.36722785270736,0.844110926180164,2.25504325859834));
#7627=CARTESIAN_POINT('Ctrl Pts',(-1.45697535334287,-0.677538247307762,
2.34942756434527));
#7628=CARTESIAN_POINT('Ctrl Pts',(-0.235547126457103,-1.58945047373708,
2.4438118700922));
#7629=CARTESIAN_POINT('Ctrl Pts',(1.19785700950514,-1.07096864650801,2.53819617583912));
#7630=CARTESIAN_POINT('Ctrl Pts',(1.55327377079637,0.411309919633114,2.63258048158605));
#7631=CARTESIAN_POINT('Ctrl Pts',(0.510852976384489,1.52343837867101,2.72696478733295));
#7632=CARTESIAN_POINT('Ctrl Pts',(-0.991299701281711,1.26457904430392,2.82134909307991));
#7633=CARTESIAN_POINT('Ctrl Pts',(-1.60135210822426,-0.1323128207854,2.91573339882681));
#7634=CARTESIAN_POINT('Ctrl Pts',(-0.770299824614874,-1.41013241834363,
3.01011770457376));
#7635=CARTESIAN_POINT('Ctrl Pts',(0.753968326190115,-1.41893164745954,3.10450201032066));
#7636=CARTESIAN_POINT('Ctrl Pts',(1.59971781403329,-0.150791818497472,3.1988863160676));
#7637=CARTESIAN_POINT('Ctrl Pts',(1.00583336157899,1.25305008112067,3.29327062181452));
#7638=CARTESIAN_POINT('Ctrl Pts',(-0.493230637487029,1.52923470903127,3.38765492756144));
#7639=CARTESIAN_POINT('Ctrl Pts',(-1.54842162351773,0.429215252389708,3.48203923330837));
#7640=CARTESIAN_POINT('Ctrl Pts',(-1.21014164638715,-1.05706785626069,3.5764235390553));
#7641=CARTESIAN_POINT('Ctrl Pts',(0.217181017787342,-1.59206396309263,3.67080784480223));
#7642=CARTESIAN_POINT('Ctrl Pts',(1.44905598384148,-0.694314059163175,3.76519215054915));
#7643=CARTESIAN_POINT('Ctrl Pts',(1.37688209988584,0.828269847373295,3.85957645629608));
#7644=CARTESIAN_POINT('Ctrl Pts',(0.0656108042523692,1.60546892821194,3.95396076204301));
#7645=CARTESIAN_POINT('Ctrl Pts',(-1.30470561785572,0.93785846894309,4.04834506778992));
#7646=CARTESIAN_POINT('Ctrl Pts',(-1.50087840470022,-0.573758896513456,
4.14272937353686));
#7647=CARTESIAN_POINT('Ctrl Pts',(-0.346365793965792,-1.56903345853926,
4.23711367928378));
#7648=CARTESIAN_POINT('Ctrl Pts',(1.11985176146982,-1.15228784995173,4.33149798503071));
#7649=CARTESIAN_POINT('Ctrl Pts',(1.57828119965777,0.301436082316522,4.42588229077763));
#7650=CARTESIAN_POINT('Ctrl Pts',(0.616368148442064,1.48388866288936,4.52026659652455));
#7651=CARTESIAN_POINT('Ctrl Pts',(-0.900233047455315,1.33094542162297,4.61465090227147));
#7652=CARTESIAN_POINT('Ctrl Pts',(-1.60668757995471,-0.0197554369790745,
4.7090352080184));
#7653=CARTESIAN_POINT('Ctrl Pts',(-0.867235871345144,-1.35267779168764,
4.80341951376534));
#7654=CARTESIAN_POINT('Ctrl Pts',(0.652667354478971,-1.46828490635015,4.89780381951226));
#7655=CARTESIAN_POINT('Ctrl Pts',(1.5852156931868,-0.26253850666854,4.99218812525918));
#7656=CARTESIAN_POINT('Ctrl Pts',(1.0911809852017,1.17947418822689,5.08657243100611));
#7657=CARTESIAN_POINT('Ctrl Pts',(-0.384840152259307,1.56004269237261,5.18095673675304));
#7658=CARTESIAN_POINT('Ctrl Pts',(-1.51453211481263,0.53668221351591,5.27534104249995));
#7659=CARTESIAN_POINT('Ctrl Pts',(-1.28125130434305,-0.969654895419948,
5.36972534824688));
#7660=CARTESIAN_POINT('Ctrl Pts',(0.105065915886374,-1.60337007932205,5.46410965399381));
#7661=CARTESIAN_POINT('Ctrl Pts',(1.39683114864801,-0.7941654210324,5.55849395974075));
#7662=CARTESIAN_POINT('Ctrl Pts',(1.43154627152773,0.729734145377444,5.65287826548766));
#7663=CARTESIAN_POINT('Ctrl Pts',(0.177969967514853,1.59692092332055,5.7472625712346));
#7664=CARTESIAN_POINT('Ctrl Pts',(-1.23576666361313,1.02699683734509,5.84164687698152));
#7665=CARTESIAN_POINT('Ctrl Pts',(-1.53740021748705,-0.46716399282643,5.93603118272843));
#7666=CARTESIAN_POINT('Ctrl Pts',(-0.455480673861307,-1.540887980073,6.03041548847536));
#7667=CARTESIAN_POINT('Ctrl Pts',(1.03633836657119,-1.22796258928818,6.1247997942223));
#7668=CARTESIAN_POINT('Ctrl Pts',(1.59552776581231,0.19012269705805,6.2191840999692));
#7669=CARTESIAN_POINT('Ctrl Pts',(0.718849649468088,1.43695938240689,6.31356840571614));
#7670=CARTESIAN_POINT('Ctrl Pts',(-0.804734544554861,1.39092163269575,6.40795271146306));
#7671=CARTESIAN_POINT('Ctrl Pts',(-1.60412976727155,0.092602940459203,6.50233701721));
#7672=CARTESIAN_POINT('Ctrl Pts',(-0.959890180152371,-1.28800496751056,
6.5967213229569));
#7673=CARTESIAN_POINT('Ctrl Pts',(0.548121242644853,-1.51151111555712,6.69110562870386));
#7674=CARTESIAN_POINT('Ctrl Pts',(1.56310784547845,-0.37065643167945,6.78549853239035));
#7675=CARTESIAN_POINT('Ctrl Pts',(1.3014618734641,0.606427672763405,6.84843000082788));
#7676=CARTESIAN_POINT('Ctrl Pts',(0.993685314990144,0.933895149917456,6.87990003401645));
#7677=CARTESIAN_POINT('Ctrl Pts',(-0.646459514637458,1.33049624488324,-0.132223047397372));
#7678=CARTESIAN_POINT('Ctrl Pts',(-1.08480930388685,1.11751150848179,-0.100761612148397));
#7679=CARTESIAN_POINT('Ctrl Pts',(-1.72748972074385,0.228459034416341,-0.037838741650446));
#7680=CARTESIAN_POINT('Ctrl Pts',(-1.13986071563865,-1.3200647398456,0.0565455640964797));
#7681=CARTESIAN_POINT('Ctrl Pts',(0.474954970979457,-1.67650645441138,0.150929869843405));
#7682=CARTESIAN_POINT('Ctrl Pts',(1.66162938758921,-0.526273512027314,0.24531417559033));
#7683=CARTESIAN_POINT('Ctrl Pts',(1.35332768345178,1.09864158048345,0.339698481337256));
#7684=CARTESIAN_POINT('Ctrl Pts',(-0.173070373162715,1.73429378997042,0.434082787084181));
#7685=CARTESIAN_POINT('Ctrl Pts',(-1.54361410933203,0.809498516568055,0.528467092831108));
#7686=CARTESIAN_POINT('Ctrl Pts',(-1.52506749024128,-0.843943917146358,
0.622851398578033));
#7687=CARTESIAN_POINT('Ctrl Pts',(-0.13403851934482,-1.73781439657543,0.717235704324959));
#7688=CARTESIAN_POINT('Ctrl Pts',(1.37760076485913,-1.06781654932485,0.811620010071883));
#7689=CARTESIAN_POINT('Ctrl Pts',(1.64950375176345,0.56316389391153,0.906004315818811));
#7690=CARTESIAN_POINT('Ctrl Pts',(0.436964811193913,1.68732445748138,1.00038862156574));
#7691=CARTESIAN_POINT('Ctrl Pts',(-1.16880967008705,1.2930174600825,1.09477292731266));
#7692=CARTESIAN_POINT('Ctrl Pts',(-1.72273848782547,-0.264917918077412,
1.18915723305959));
#7693=CARTESIAN_POINT('Ctrl Pts',(-0.7263227793451,-1.58444401519218,1.28354153880651));
#7694=CARTESIAN_POINT('Ctrl Pts',(0.9237322219861,-1.47808242332004,1.37792584455344));
#7695=CARTESIAN_POINT('Ctrl Pts',(1.74249311507829,-0.0415497454832925,
1.47231015030036));
#7696=CARTESIAN_POINT('Ctrl Pts',(0.993132214199591,1.43237454264688,1.56669445604729));
#7697=CARTESIAN_POINT('Ctrl Pts',(-0.649978044897315,1.61726223995226,1.66107876179422));
#7698=CARTESIAN_POINT('Ctrl Pts',(-1.70815363161769,0.346727174142455,1.75546306754114));
#7699=CARTESIAN_POINT('Ctrl Pts',(-1.22911062769304,-1.2358380170301,1.84984737328807));
#7700=CARTESIAN_POINT('Ctrl Pts',(0.356045810658149,-1.70623560713348,1.94423167903499));
#7701=CARTESIAN_POINT('Ctrl Pts',(1.62078597105695,-0.6411406968694,2.03861598478192));
#7702=CARTESIAN_POINT('Ctrl Pts',(1.4269323242515,1.00093591055773,2.13300029052884));
#7703=CARTESIAN_POINT('Ctrl Pts',(-0.0510604281759689,1.74224033688597,
2.22738459627577));
#7704=CARTESIAN_POINT('Ctrl Pts',(-1.48310237355857,0.915650537462024,2.3217689020227));
#7705=CARTESIAN_POINT('Ctrl Pts',(-1.58045610355311,-0.734960585222904,
2.41615320776962));
#7706=CARTESIAN_POINT('Ctrl Pts',(-0.255510083152334,-1.72415868034384,
2.51053751351654));
#7707=CARTESIAN_POINT('Ctrl Pts',(1.29937710855069,-1.16173477485675,2.60492181926348));
#7708=CARTESIAN_POINT('Ctrl Pts',(1.68491594995867,0.446169025059073,2.69930612501039));
#7709=CARTESIAN_POINT('Ctrl Pts',(0.554148498595194,1.65255196557264,2.79369043075733));
#7710=CARTESIAN_POINT('Ctrl Pts',(-1.075313772293,1.37175393146487,2.88807473650425));
#7711=CARTESIAN_POINT('Ctrl Pts',(-1.7370689954184,-0.143526522057367,2.98245904225118));
#7712=CARTESIAN_POINT('Ctrl Pts',(-0.835583839208558,-1.52964316264918,
3.0768433479981));
#7713=CARTESIAN_POINT('Ctrl Pts',(0.817868222876148,-1.53918813904903,3.17122765374503));
#7714=CARTESIAN_POINT('Ctrl Pts',(1.7352961924515,-0.163571641320779,3.26561195949195));
#7715=CARTESIAN_POINT('Ctrl Pts',(1.09107918113888,1.35924787212158,3.35999626523888));
#7716=CARTESIAN_POINT('Ctrl Pts',(-0.535032641209211,1.65883954324172,3.4543805709858));
#7717=CARTESIAN_POINT('Ctrl Pts',(-1.67965257624115,0.465591860439508,3.54876487673272));
#7718=CARTESIAN_POINT('Ctrl Pts',(-1.31270288602219,-1.14665587270498,3.64314918247966));
#7719=CARTESIAN_POINT('Ctrl Pts',(0.235587420439429,-1.7269936666695,3.73753348822658));
#7720=CARTESIAN_POINT('Ctrl Pts',(1.57186555613167,-0.753158171186272,3.83191779397351));
#7721=CARTESIAN_POINT('Ctrl Pts',(1.49357483202773,0.898466904513287,3.92630209972043));
#7722=CARTESIAN_POINT('Ctrl Pts',(0.0711714139856785,1.74153472180275,4.02068640546736));
#7723=CARTESIAN_POINT('Ctrl Pts',(-1.41528128965875,1.01734331888955,4.11507071121428));
#7724=CARTESIAN_POINT('Ctrl Pts',(-1.62808000146129,-0.62238578564972,4.20945501696121));
#7725=CARTESIAN_POINT('Ctrl Pts',(-0.375720791624429,-1.70201129383405,
4.30383932270812));
#7726=CARTESIAN_POINT('Ctrl Pts',(1.21476080390027,-1.24994589738797,4.39822362845507));
#7727=CARTESIAN_POINT('Ctrl Pts',(1.71204279427179,0.326983222492551,4.49260793420197));
#7728=CARTESIAN_POINT('Ctrl Pts',(0.668606232772531,1.60965035467203,4.58699223994891));
#7729=CARTESIAN_POINT('Ctrl Pts',(-0.976529088983251,1.44374495441797,4.68137654569583));
#7730=CARTESIAN_POINT('Ctrl Pts',(-1.74285665602802,-0.0214297385884319,
4.77576085144276));
#7731=CARTESIAN_POINT('Ctrl Pts',(-0.940735354886333,-1.46731917400552,
4.87014515718968));
#7732=CARTESIAN_POINT('Ctrl Pts',(0.707981848566931,-1.59272415739343,4.96452946293661));
#7733=CARTESIAN_POINT('Ctrl Pts',(1.71956499607009,-0.28478902153699,5.05891376868354));
#7734=CARTESIAN_POINT('Ctrl Pts',(1.18366013823523,1.27943631681177,5.15329807443046));
#7735=CARTESIAN_POINT('Ctrl Pts',(-0.417455906947926,1.6922585473438,5.24768238017739));
#7736=CARTESIAN_POINT('Ctrl Pts',(-1.64289088308245,0.582166800607521,5.34206668592431));
#7737=CARTESIAN_POINT('Ctrl Pts',(-1.38983918944704,-1.05183453810009,5.43645099167124));
#7738=CARTESIAN_POINT('Ctrl Pts',(0.113970402901476,-1.73925799246011,5.53083529741816));
#7739=CARTESIAN_POINT('Ctrl Pts',(1.51521459127547,-0.861472079141013,5.62521960316509));
#7740=CARTESIAN_POINT('Ctrl Pts',(1.55287187059388,0.791580160492583,5.71960390891201));
#7741=CARTESIAN_POINT('Ctrl Pts',(0.193053177435471,1.73226226124066,5.81398821465895));
#7742=CARTESIAN_POINT('Ctrl Pts',(-1.34049966019928,1.1140362918204,5.90837252040586));
#7743=CARTESIAN_POINT('Ctrl Pts',(-1.66769709024686,-0.506756811039214,
6.00275682615279));
#7744=CARTESIAN_POINT('Ctrl Pts',(-0.494083314040241,-1.67148044571272,
6.09714113189972));
#7745=CARTESIAN_POINT('Ctrl Pts',(1.1241695290423,-1.33203417938579,6.19152543764664));
#7746=CARTESIAN_POINT('Ctrl Pts',(1.73075103163608,0.20623586823205,6.28590974339357));
#7747=CARTESIAN_POINT('Ctrl Pts',(0.779773187948709,1.55874375038136,6.38029404914049));
#7748=CARTESIAN_POINT('Ctrl Pts',(-0.872936951036021,1.50880423537318,6.47467835488741));
#7749=CARTESIAN_POINT('Ctrl Pts',(-1.74008206505257,0.100451172437426,6.56906266063435));
#7750=CARTESIAN_POINT('Ctrl Pts',(-1.04124224921292,-1.3971652352514,6.66344696638127));
#7751=CARTESIAN_POINT('Ctrl Pts',(0.594575303856428,-1.63961384980852,6.7578312721282));
#7752=CARTESIAN_POINT('Ctrl Pts',(1.69558347657019,-0.40207009571229,6.8522241758147));
#7753=CARTESIAN_POINT('Ctrl Pts',(1.41176263327905,0.657823287527416,6.91515564425223));
#7754=CARTESIAN_POINT('Ctrl Pts',(1.07790157018373,1.01304410289385,6.9466256774408));
#7755=CARTESIAN_POINT('Ctrl Pts',(-0.696967279875932,1.43444767643566,-0.0654974039730188));
#7756=CARTESIAN_POINT('Ctrl Pts',(-1.1695652590683,1.20482248100781,-0.0340359687240437));
#7757=CARTESIAN_POINT('Ctrl Pts',(-1.86245818093606,0.246308497554627,0.0288869017739064));
#7758=CARTESIAN_POINT('Ctrl Pts',(-1.22891782768739,-1.42320115979157,0.123271207520832));
#7759=CARTESIAN_POINT('Ctrl Pts',(0.512063117166348,-1.80749160120389,0.217655513267758));
#7760=CARTESIAN_POINT('Ctrl Pts',(1.79145219183517,-0.567391166566931,0.312039819014683));
#7761=CARTESIAN_POINT('Ctrl Pts',(1.45906293118009,1.18447824893965,0.406424124761609));
#7762=CARTESIAN_POINT('Ctrl Pts',(-0.186592330190968,1.86979385086363,0.500808430508534));
#7763=CARTESIAN_POINT('Ctrl Pts',(-1.66421640118114,0.872744489610393,0.59519273625546));
#7764=CARTESIAN_POINT('Ctrl Pts',(-1.64422073808718,-0.909881103120909,
0.689577042002386));
#7765=CARTESIAN_POINT('Ctrl Pts',(-0.144510924676781,-1.87358952182748,
0.78396134774931));
#7766=CARTESIAN_POINT('Ctrl Pts',(1.48523246405823,-1.15124486365837,0.878345653496237));
#7767=CARTESIAN_POINT('Ctrl Pts',(1.77837918227017,0.607163787331645,0.972729959243162));
#7768=CARTESIAN_POINT('Ctrl Pts',(0.471104793051308,1.81915481290187,1.06711426499009));
#7769=CARTESIAN_POINT('Ctrl Pts',(-1.26012855872361,1.3940406809407,1.16149857073701));
#7770=CARTESIAN_POINT('Ctrl Pts',(-1.85733573504703,-0.285615907217876,
1.25588287648394));
#7771=CARTESIAN_POINT('Ctrl Pts',(-0.783070247045533,-1.70823634021925,
1.35026718223087));
#7772=CARTESIAN_POINT('Ctrl Pts',(0.995903253821642,-1.59356473636487,1.44465148797779));
#7773=CARTESIAN_POINT('Ctrl Pts',(1.8786337877628,-0.0447960196011254,1.53903579372472));
#7774=CARTESIAN_POINT('Ctrl Pts',(1.070725454905,1.54428570722175,1.63342009947164));
#7775=CARTESIAN_POINT('Ctrl Pts',(-0.700760712270145,1.74361864695846,1.72780440521857));
#7776=CARTESIAN_POINT('Ctrl Pts',(-1.84161136665526,0.373816905698525,1.82218871096549));
#7777=CARTESIAN_POINT('Ctrl Pts',(-1.32514081926731,-1.33239381831945,1.91657301671242));
#7778=CARTESIAN_POINT('Ctrl Pts',(0.383863605603818,-1.83954348726417,2.01095732245934));
#7779=CARTESIAN_POINT('Ctrl Pts',(1.74741768653858,-0.691232903835339,2.10534162820627));
#7780=CARTESIAN_POINT('Ctrl Pts',(1.53841828928508,1.07913885265157,2.19972593395319));
#7781=CARTESIAN_POINT('Ctrl Pts',(-0.0550497702165604,1.87836126005592,
2.29411023970012));
#7782=CARTESIAN_POINT('Ctrl Pts',(-1.5989768944098,0.987190148743883,2.38849454544705));
#7783=CARTESIAN_POINT('Ctrl Pts',(-1.70393685376336,-0.792382923138043,
2.48287885119397));
#7784=CARTESIAN_POINT('Ctrl Pts',(-0.275473039847566,-1.85886688695062,
2.5772631569409));
#7785=CARTESIAN_POINT('Ctrl Pts',(1.40089720759624,-1.25250090320548,2.67164746268782));
#7786=CARTESIAN_POINT('Ctrl Pts',(1.81655812912099,0.481028130485029,2.76603176843475));
#7787=CARTESIAN_POINT('Ctrl Pts',(0.597444020805899,1.78166555247427,2.86041607418167));
#7788=CARTESIAN_POINT('Ctrl Pts',(-1.15932784330429,1.47892881862582,2.9548003799286));
#7789=CARTESIAN_POINT('Ctrl Pts',(-1.87278588261255,-0.154740223329332,
3.04918468567552));
#7790=CARTESIAN_POINT('Ctrl Pts',(-0.900867853802242,-1.64915390695474,
3.14356899142245));
#7791=CARTESIAN_POINT('Ctrl Pts',(0.881768119562182,-1.65944463063851,3.23795329716937));
#7792=CARTESIAN_POINT('Ctrl Pts',(1.87087457086971,-0.176351464144087,3.3323376029163));
#7793=CARTESIAN_POINT('Ctrl Pts',(1.17632500069877,1.46544566312249,3.42672190866323));
#7794=CARTESIAN_POINT('Ctrl Pts',(-0.576834644931392,1.78844437745218,3.52110621441015));
#7795=CARTESIAN_POINT('Ctrl Pts',(-1.81088352896457,0.501968468489308,3.61549052015708));
#7796=CARTESIAN_POINT('Ctrl Pts',(-1.41526412565724,-1.23624388914925,3.709874825904));
#7797=CARTESIAN_POINT('Ctrl Pts',(0.253993823091515,-1.86192337024639,3.80425913165093));
#7798=CARTESIAN_POINT('Ctrl Pts',(1.69467512842186,-0.81200228320937,3.89864343739786));
#7799=CARTESIAN_POINT('Ctrl Pts',(1.61026756416961,0.968663961653281,3.99302774314478));
#7800=CARTESIAN_POINT('Ctrl Pts',(0.0767320237189894,1.87760051539355,4.08741204889171));
#7801=CARTESIAN_POINT('Ctrl Pts',(-1.52585696146177,1.09682816883599,4.18179635463863));
#7802=CARTESIAN_POINT('Ctrl Pts',(-1.75528159822236,-0.671012674785984,
4.27618066038555));
#7803=CARTESIAN_POINT('Ctrl Pts',(-0.405075789283068,-1.83498912912884,
4.37056496613248));
#7804=CARTESIAN_POINT('Ctrl Pts',(1.30966984633074,-1.34760394482421,4.46494927187941));
#7805=CARTESIAN_POINT('Ctrl Pts',(1.84580438888581,0.35253036266858,4.55933357762632));
#7806=CARTESIAN_POINT('Ctrl Pts',(0.720844317102997,1.7354120464547,4.65371788337327));
#7807=CARTESIAN_POINT('Ctrl Pts',(-1.05282513051118,1.55654448721296,4.74810218912018));
#7808=CARTESIAN_POINT('Ctrl Pts',(-1.87902573210135,-0.023104040197789,
4.84248649486711));
#7809=CARTESIAN_POINT('Ctrl Pts',(-1.01423483842752,-1.58196055632341,4.93687080061403));
#7810=CARTESIAN_POINT('Ctrl Pts',(0.763296342654892,-1.7171634084367,5.03125510636096));
#7811=CARTESIAN_POINT('Ctrl Pts',(1.85391429895339,-0.307039536405439,5.12563941210788));
#7812=CARTESIAN_POINT('Ctrl Pts',(1.27613929126875,1.37939844539666,5.22002371785481));
#7813=CARTESIAN_POINT('Ctrl Pts',(-0.450071661636544,1.82447440231499,5.31440802360174));
#7814=CARTESIAN_POINT('Ctrl Pts',(-1.77124965135225,0.627651387699125,5.40879232934866));
#7815=CARTESIAN_POINT('Ctrl Pts',(-1.49842707455103,-1.13401418078021,5.50317663509559));
#7816=CARTESIAN_POINT('Ctrl Pts',(0.122874889916577,-1.87514590559817,5.59756094084251));
#7817=CARTESIAN_POINT('Ctrl Pts',(1.63359803390294,-0.928778737249626,5.69194524658944));
#7818=CARTESIAN_POINT('Ctrl Pts',(1.67419746966002,0.853426175607722,5.78632955233636));
#7819=CARTESIAN_POINT('Ctrl Pts',(0.208136387356091,1.86760359916079,5.88071385808329));
#7820=CARTESIAN_POINT('Ctrl Pts',(-1.44523265678541,1.20107574629571,5.97509816383021));
#7821=CARTESIAN_POINT('Ctrl Pts',(-1.79799396300668,-0.546349629251995,
6.06948246957714));
#7822=CARTESIAN_POINT('Ctrl Pts',(-0.532685954219177,-1.80207291135245,
6.16386677532407));
#7823=CARTESIAN_POINT('Ctrl Pts',(1.21200069151341,-1.4361057694834,6.25825108107099));
#7824=CARTESIAN_POINT('Ctrl Pts',(1.86597429745986,0.222349039406046,6.35263538681792));
#7825=CARTESIAN_POINT('Ctrl Pts',(0.84069672642933,1.68052811835584,6.44701969256484));
#7826=CARTESIAN_POINT('Ctrl Pts',(-0.941139357517183,1.62668683805062,6.54140399831177));
#7827=CARTESIAN_POINT('Ctrl Pts',(-1.87603436283358,0.108299404415651,6.6357883040587));
#7828=CARTESIAN_POINT('Ctrl Pts',(-1.12259431827347,-1.50632550299225,6.73017260980562));
#7829=CARTESIAN_POINT('Ctrl Pts',(0.641029365068003,-1.76771658405992,6.82455691555255));
#7830=CARTESIAN_POINT('Ctrl Pts',(1.82805910766192,-0.433483759745132,6.91894981923906));
#7831=CARTESIAN_POINT('Ctrl Pts',(1.52206339309401,0.709218902291427,6.98188128767659));
#7832=CARTESIAN_POINT('Ctrl Pts',(1.16211782537732,1.09219305587025,7.01335132086515));
#7833=CARTESIAN_POINT('Ctrl Pts',(-0.747475045114406,1.53839910798808,0.00122823945133365));
#7834=CARTESIAN_POINT('Ctrl Pts',(-1.25432121424975,1.29213345353384,0.0326896747003088));
#7835=CARTESIAN_POINT('Ctrl Pts',(-1.99742664112827,0.264157960692912,0.0956125451982589));
#7836=CARTESIAN_POINT('Ctrl Pts',(-1.31797493973614,-1.52633757973754,0.189996850945185));
#7837=CARTESIAN_POINT('Ctrl Pts',(0.549171263353243,-1.93847674799641,0.28438115669211));
#7838=CARTESIAN_POINT('Ctrl Pts',(1.92127499608112,-0.608508821106544,0.378765462439036));
#7839=CARTESIAN_POINT('Ctrl Pts',(1.56479817890842,1.27031491739583,0.473149768185962));
#7840=CARTESIAN_POINT('Ctrl Pts',(-0.200114287219223,2.00529391175686,0.567534073932887));
#7841=CARTESIAN_POINT('Ctrl Pts',(-1.78481869303027,0.935990462652723,0.661918379679812));
#7842=CARTESIAN_POINT('Ctrl Pts',(-1.7633739859331,-0.975818289095456,0.756302685426739));
#7843=CARTESIAN_POINT('Ctrl Pts',(-0.154983330008743,-2.00936464707954,
0.850686991173664));
#7844=CARTESIAN_POINT('Ctrl Pts',(1.59286416325733,-1.23467317799189,0.945071296920589));
#7845=CARTESIAN_POINT('Ctrl Pts',(1.90725461277688,0.65116368075176,1.03945560266751));
#7846=CARTESIAN_POINT('Ctrl Pts',(0.505244774908705,1.95098516832236,1.13383990841444));
#7847=CARTESIAN_POINT('Ctrl Pts',(-1.35144744736016,1.4950639017989,1.22822421416136));
#7848=CARTESIAN_POINT('Ctrl Pts',(-1.99193298226858,-0.306313896358341,
1.32260851990829));
#7849=CARTESIAN_POINT('Ctrl Pts',(-0.839817714745969,-1.83202866524631,
1.41699282565521));
#7850=CARTESIAN_POINT('Ctrl Pts',(1.06807428565718,-1.70904704940972,1.51137713140214));
#7851=CARTESIAN_POINT('Ctrl Pts',(2.01477446044731,-0.0480422937189565,
1.60576143714906));
#7852=CARTESIAN_POINT('Ctrl Pts',(1.14831869561041,1.65619687179661,1.70014574289599));
#7853=CARTESIAN_POINT('Ctrl Pts',(-0.751543379642974,1.86997505396467,1.79453004864291));
#7854=CARTESIAN_POINT('Ctrl Pts',(-1.97506910169283,0.400906637254589,1.88891435438984));
#7855=CARTESIAN_POINT('Ctrl Pts',(-1.42117101084157,-1.42894961960879,1.98329866013677));
#7856=CARTESIAN_POINT('Ctrl Pts',(0.411681400549486,-1.97285136739486,2.07768296588369));
#7857=CARTESIAN_POINT('Ctrl Pts',(1.8740494020202,-0.741325110801277,2.17206727163062));
#7858=CARTESIAN_POINT('Ctrl Pts',(1.64990425431865,1.15734179474542,2.26645157737754));
#7859=CARTESIAN_POINT('Ctrl Pts',(-0.0590391122571503,2.01448218322587,
2.36083588312447));
#7860=CARTESIAN_POINT('Ctrl Pts',(-1.71485141526102,1.05872976002574,2.45522018887139));
#7861=CARTESIAN_POINT('Ctrl Pts',(-1.8274176039736,-0.849805261053182,2.54960449461832));
#7862=CARTESIAN_POINT('Ctrl Pts',(-0.295435996542797,-1.99357509355738,
2.64398880036524));
#7863=CARTESIAN_POINT('Ctrl Pts',(1.50241730664178,-1.34326703155423,2.73837310611218));
#7864=CARTESIAN_POINT('Ctrl Pts',(1.9482003082833,0.515887235910986,2.83275741185909));
#7865=CARTESIAN_POINT('Ctrl Pts',(0.640739543016601,1.9107791393759,2.92714171760603));
#7866=CARTESIAN_POINT('Ctrl Pts',(-1.24334191431558,1.58610370578677,3.02152602335295));
#7867=CARTESIAN_POINT('Ctrl Pts',(-2.0085027698067,-0.165953924601296,3.11591032909987));
#7868=CARTESIAN_POINT('Ctrl Pts',(-0.966151868395926,-1.76866465126028,
3.2102946348468));
#7869=CARTESIAN_POINT('Ctrl Pts',(0.945668016248215,-1.779701122228,3.30467894059372));
#7870=CARTESIAN_POINT('Ctrl Pts',(2.00645294928792,-0.189131286967392,3.39906324634065));
#7871=CARTESIAN_POINT('Ctrl Pts',(1.26157082025866,1.5716434541234,3.49344755208758));
#7872=CARTESIAN_POINT('Ctrl Pts',(-0.618636648653572,1.91804921166265,3.58783185783451));
#7873=CARTESIAN_POINT('Ctrl Pts',(-1.94211448168799,0.538345076539106,3.68221616358144));
#7874=CARTESIAN_POINT('Ctrl Pts',(-1.51782536529229,-1.32583190559354,3.77660046932835));
#7875=CARTESIAN_POINT('Ctrl Pts',(0.2724002257436,-1.99685307382326,3.87098477507528));
#7876=CARTESIAN_POINT('Ctrl Pts',(1.81748470071205,-0.870846395232466,3.9653690808222));
#7877=CARTESIAN_POINT('Ctrl Pts',(1.72696029631149,1.03886101879327,4.05975338656913));
#7878=CARTESIAN_POINT('Ctrl Pts',(0.0822926334523,2.01366630898437,4.15413769231605));
#7879=CARTESIAN_POINT('Ctrl Pts',(-1.63643263326479,1.17631301878244,4.24852199806298));
#7880=CARTESIAN_POINT('Ctrl Pts',(-1.88248319498343,-0.719639563922248,
4.3429063038099));
#7881=CARTESIAN_POINT('Ctrl Pts',(-0.434430786941708,-1.96796696442363,
4.43729060955683));
#7882=CARTESIAN_POINT('Ctrl Pts',(1.40457888876119,-1.44526199226046,4.53167491530376));
#7883=CARTESIAN_POINT('Ctrl Pts',(1.97956598349983,0.378077502844609,4.62605922105068));
#7884=CARTESIAN_POINT('Ctrl Pts',(0.773082401433464,1.86117373823736,4.72044352679761));
#7885=CARTESIAN_POINT('Ctrl Pts',(-1.12912117203912,1.66934402000796,4.81482783254453));
#7886=CARTESIAN_POINT('Ctrl Pts',(-2.01519480817465,-0.0247783418071453,
4.90921213829146));
#7887=CARTESIAN_POINT('Ctrl Pts',(-1.08773432196871,-1.6966019386413,5.00359644403838));
#7888=CARTESIAN_POINT('Ctrl Pts',(0.818610836742852,-1.84160265947997,5.09798074978531));
#7889=CARTESIAN_POINT('Ctrl Pts',(1.98826360183667,-0.32929005127389,5.19236505553224));
#7890=CARTESIAN_POINT('Ctrl Pts',(1.36861844430227,1.47936057398154,5.28674936127916));
#7891=CARTESIAN_POINT('Ctrl Pts',(-0.48268741632516,1.95669025728617,5.38113366702608));
#7892=CARTESIAN_POINT('Ctrl Pts',(-1.89960841962207,0.673135974790736,5.47551797277302));
#7893=CARTESIAN_POINT('Ctrl Pts',(-1.60701495965502,-1.21619382346035,5.56990227851994));
#7894=CARTESIAN_POINT('Ctrl Pts',(0.13177937693168,-2.01103381873623,5.66428658426686));
#7895=CARTESIAN_POINT('Ctrl Pts',(1.7519814765304,-0.99608539535824,5.7586708900138));
#7896=CARTESIAN_POINT('Ctrl Pts',(1.79552306872616,0.915272190722859,5.85305519576071));
#7897=CARTESIAN_POINT('Ctrl Pts',(0.223219597276707,2.00294493708091,5.94743950150766));
#7898=CARTESIAN_POINT('Ctrl Pts',(-1.54996565337156,1.28811520077101,6.04182380725456));
#7899=CARTESIAN_POINT('Ctrl Pts',(-1.92829083576649,-0.585942447464776,
6.13620811300149));
#7900=CARTESIAN_POINT('Ctrl Pts',(-0.57128859439811,-1.93266537699218,6.23059241874842));
#7901=CARTESIAN_POINT('Ctrl Pts',(1.29983185398451,-1.54017735958102,6.32497672449534));
#7902=CARTESIAN_POINT('Ctrl Pts',(2.00119756328365,0.238462210580048,6.41936103024226));
#7903=CARTESIAN_POINT('Ctrl Pts',(0.901620264909948,1.8023124863303,6.5137453359892));
#7904=CARTESIAN_POINT('Ctrl Pts',(-1.00934176399834,1.74456944072806,6.60812964173611));
#7905=CARTESIAN_POINT('Ctrl Pts',(-2.0119866606146,0.116147636393871,6.70251394748306));
#7906=CARTESIAN_POINT('Ctrl Pts',(-1.20394638733402,-1.61548577073308,6.79689825322996));
#7907=CARTESIAN_POINT('Ctrl Pts',(0.687483426279577,-1.89581931831132,6.8912825589769));
#7908=CARTESIAN_POINT('Ctrl Pts',(1.96053473875365,-0.46489742377797,6.98567546266341));
#7909=CARTESIAN_POINT('Ctrl Pts',(1.63236415290896,0.760614517055437,7.04860693110094));
#7910=CARTESIAN_POINT('Ctrl Pts',(1.24633408057091,1.17134200884666,7.08007696428951));
#7911=CARTESIAN_POINT('Ctrl Pts',(0.433521463884974,-1.65487835139843,6.88122480138926));
#7912=CARTESIAN_POINT('Ctrl Pts',(0.48286633167622,-1.63704432698362,6.88122480138927));
#7913=CARTESIAN_POINT('Ctrl Pts',(0.531233565484471,-1.61684089219081,6.88122480138927));
#7914=CARTESIAN_POINT('Ctrl Pts',(0.578448771240116,-1.59422718307761,6.88122480138927));
#7915=CARTESIAN_POINT('Ctrl Pts',(0.637301800459365,-1.56603954178929,6.88122480138927));
#7916=CARTESIAN_POINT('Ctrl Pts',(0.694366366669772,-1.53410742466645,6.88122480138927));
#7917=CARTESIAN_POINT('Ctrl Pts',(0.749419640704226,-1.49872451372066,6.88122480138927));
#7918=CARTESIAN_POINT('Ctrl Pts',(0.77114866472208,-1.48475920220656,6.88122480138927));
#7919=CARTESIAN_POINT('Ctrl Pts',(0.792563942974927,-1.47025593156819,6.88122480138927));
#7920=CARTESIAN_POINT('Ctrl Pts',(0.813649982189817,-1.45523144121435,6.88122480138927));
#7921=CARTESIAN_POINT('Ctrl Pts',(0.826217216190941,-1.44627687729175,6.88122480138927));
#7922=CARTESIAN_POINT('Ctrl Pts',(0.838668448552751,-1.43713623173645,6.88122480138927));
#7923=CARTESIAN_POINT('Ctrl Pts',(0.850984238037051,-1.42782560626945,6.88122480138927));
#7924=CARTESIAN_POINT('Ctrl Pts',(0.902467037297749,-1.3889050756352,6.88122480138927));
#7925=CARTESIAN_POINT('Ctrl Pts',(0.95165412885067,-1.34696984463084,6.88122480138927));
#7926=CARTESIAN_POINT('Ctrl Pts',(0.998333866062454,-1.30231142297158,6.88122480138927));
#7927=CARTESIAN_POINT('Ctrl Pts',(1.03120466603183,-1.27086398703916,6.88122480138927));
#7928=CARTESIAN_POINT('Ctrl Pts',(1.06283139573338,-1.23806535986098,6.88122480138927));
#7929=CARTESIAN_POINT('Ctrl Pts',(1.09312668212505,-1.204009648788,6.88122480138927));
#7930=CARTESIAN_POINT('Ctrl Pts',(1.11086405824911,-1.18407060782089,6.88122480138928));
#7931=CARTESIAN_POINT('Ctrl Pts',(1.12814480788324,-1.16370055148135,6.88122480138927));
#7932=CARTESIAN_POINT('Ctrl Pts',(1.14494937865368,-1.14291778130075,6.88122480138928));
#7933=CARTESIAN_POINT('Ctrl Pts',(1.15221458967818,-1.13393265379595,6.88122480138928));
#7934=CARTESIAN_POINT('Ctrl Pts',(1.15938472523217,-1.12487785140287,6.88122480138927));
#7935=CARTESIAN_POINT('Ctrl Pts',(1.16645787983334,-1.11575613827896,6.88122480138927));
#7936=CARTESIAN_POINT('Ctrl Pts',(1.20502462160414,-1.06601952507116,6.88122480138927));
#7937=CARTESIAN_POINT('Ctrl Pts',(1.2407199156978,-1.01428551684517,6.88122480138927));
#7938=CARTESIAN_POINT('Ctrl Pts',(1.27334306155911,-0.960820138530249,6.88122480138927));
#7939=CARTESIAN_POINT('Ctrl Pts',(1.30592057494354,-0.907429546308939,6.88122480138927));
#7940=CARTESIAN_POINT('Ctrl Pts',(1.33543504029667,-0.852311439716943,6.88122480138928));
#7941=CARTESIAN_POINT('Ctrl Pts',(1.36163634733777,-0.795715456114972,6.88122480138927));
#7942=CARTESIAN_POINT('Ctrl Pts',(1.38783765437887,-0.739119472513,6.88122480138927));
#7943=CARTESIAN_POINT('Ctrl Pts',(1.41072631426025,-0.681044662516224,6.88122480138927));
#7944=CARTESIAN_POINT('Ctrl Pts',(1.42999425119658,-0.621739849690903,6.88122480138927));
#7945=CARTESIAN_POINT('Ctrl Pts',(1.43427223611634,-0.608572633305774,6.88122480138927));
#7946=CARTESIAN_POINT('Ctrl Pts',(1.43837246784893,-0.595341002512054,6.88122480138927));
#7947=CARTESIAN_POINT('Ctrl Pts',(1.44228388835249,-0.582073867848763,6.88122480138927));
#7948=CARTESIAN_POINT('Ctrl Pts',(1.45898642628307,-0.525420583001915,6.88122480138927));
#7949=CARTESIAN_POINT('Ctrl Pts',(1.47228074592207,-0.468032401322888,6.88122480138927));
#7950=CARTESIAN_POINT('Ctrl Pts',(1.4819610710342,-0.410128498806204,6.88122480138927));
#7951=CARTESIAN_POINT('Ctrl Pts',(1.48501607616399,-0.391854658085531,6.88122480138927));
#7952=CARTESIAN_POINT('Ctrl Pts',(1.48771075601926,-0.373529425782789,6.88122480138927));
#7953=CARTESIAN_POINT('Ctrl Pts',(1.49003754927256,-0.355159679252195,6.88122480138927));
#7954=CARTESIAN_POINT('Ctrl Pts',(1.49778245475607,-0.294014603112158,6.88122480138927));
#7955=CARTESIAN_POINT('Ctrl Pts',(1.5014555591722,-0.23237502353427,6.88122480138927));
#7956=CARTESIAN_POINT('Ctrl Pts',(1.50117058949863,-0.17058848658511,6.88122480138927));
#7957=CARTESIAN_POINT('Ctrl Pts',(1.5010450609477,-0.143371645042982,6.88122480138927));
#7958=CARTESIAN_POINT('Ctrl Pts',(1.50015079106509,-0.116126514557446,6.88122480138927));
#7959=CARTESIAN_POINT('Ctrl Pts',(1.49849429649857,-0.0888842916021443,
6.88122480138927));
#7960=CARTESIAN_POINT('Ctrl Pts',(1.49741398382498,-0.0711177867731435,
6.88122480138927));
#7961=CARTESIAN_POINT('Ctrl Pts',(1.49600944105652,-0.0533525402256336,
6.88122480138926));
#7962=CARTESIAN_POINT('Ctrl Pts',(1.49428207131083,-0.0355975031972548,
6.88122480138926));
#7963=CARTESIAN_POINT('Ctrl Pts',(1.49320087544153,-0.0244842642729668,
6.88122480138926));
#7964=CARTESIAN_POINT('Ctrl Pts',(1.49199294904392,-0.0133738365360173,
6.88122480138926));
#7965=CARTESIAN_POINT('Ctrl Pts',(1.49066097672539,-0.00228582989250978,
6.88122480138926));
#7966=CARTESIAN_POINT('Ctrl Pts',(1.48365926906569,0.0559999017000902,6.88122480138927));
#7967=CARTESIAN_POINT('Ctrl Pts',(1.47322434547187,0.113778347564274,6.88122480138927));
#7968=CARTESIAN_POINT('Ctrl Pts',(1.4594842086581,0.170755138432216,6.88122480138927));
#7969=CARTESIAN_POINT('Ctrl Pts',(1.44587229152792,0.227200235460672,6.88122480138927));
#7970=CARTESIAN_POINT('Ctrl Pts',(1.42901593858198,0.282859526726203,6.88122480138927));
#7971=CARTESIAN_POINT('Ctrl Pts',(1.40899511525678,0.337423685152158,6.88122480138927));
#7972=CARTESIAN_POINT('Ctrl Pts',(1.38913180150897,0.391558571644822,6.88122480138927));
#7973=CARTESIAN_POINT('Ctrl Pts',(1.36615305512817,0.444616362809891,6.88122480138927));
#7974=CARTESIAN_POINT('Ctrl Pts',(1.34010169134689,0.49625853363983,6.88122480138927));
#7975=CARTESIAN_POINT('Ctrl Pts',(1.3336683238708,0.509011534404064,6.88122480138926));
#7976=CARTESIAN_POINT('Ctrl Pts',(1.3270447516601,0.521682626600951,6.88122480138927));
#7977=CARTESIAN_POINT('Ctrl Pts',(1.32024668026891,0.534238885958241,6.88122480138927));
#7978=CARTESIAN_POINT('Ctrl Pts',(1.29340017822458,0.583825249958668,6.88122480138927));
#7979=CARTESIAN_POINT('Ctrl Pts',(1.26380097432666,0.631696741779596,6.88122480138926));
#7980=CARTESIAN_POINT('Ctrl Pts',(1.23153271624108,0.677572305460653,6.88122480138926));
#7981=CARTESIAN_POINT('Ctrl Pts',(1.2003110151207,0.721959986201897,6.88122480138927));
#7982=CARTESIAN_POINT('Ctrl Pts',(1.16658992943844,0.764479679279131,6.88122480138927));
#7983=CARTESIAN_POINT('Ctrl Pts',(1.13041488599057,0.804840324534032,6.88122480138927));
#7984=CARTESIAN_POINT('Ctrl Pts',(1.09445590942473,0.844959903077031,6.88122480138927));
#7985=CARTESIAN_POINT('Ctrl Pts',(1.0560717388421,0.882946797134589,6.88122480138927));
#7986=CARTESIAN_POINT('Ctrl Pts',(1.01528449697062,0.91846928819733,6.88122480138927));
#7987=CARTESIAN_POINT('Ctrl Pts',(1.00879798113654,0.924118535122891,6.88122480138927));
#7988=CARTESIAN_POINT('Ctrl Pts',(1.00225064991045,0.929705347318732,6.88122480138927));
#7989=CARTESIAN_POINT('Ctrl Pts',(0.995642551412613,0.935228266155693,6.88122480138927));
#7990=CARTESIAN_POINT('Ctrl Pts',(-0.795414167084174,-1.11297035801352,
-9.15933995315754E-16));
#7991=CARTESIAN_POINT('Ctrl Pts',(-0.832947493180536,-1.09280171046842,
-4.40215524741542E-15));
#7992=CARTESIAN_POINT('Ctrl Pts',(-0.86936688691735,-1.07084409499352,-3.25857603395726E-15));
#7993=CARTESIAN_POINT('Ctrl Pts',(-0.904527909503487,-1.04713770592261,
-3.07219527595493E-15));
#7994=CARTESIAN_POINT('Ctrl Pts',(-0.949274147286779,-1.01696873914267,
-2.93443362582291E-15));
#7995=CARTESIAN_POINT('Ctrl Pts',(-0.991983854002586,-0.983969661606057,
-3.24217105220443E-15));
#7996=CARTESIAN_POINT('Ctrl Pts',(-1.0325919733568,-0.948460486377737,-3.64291929955129E-15));
#7997=CARTESIAN_POINT('Ctrl Pts',(-1.07423105118419,-0.912049804611821,
-4.05384173885249E-15));
#7998=CARTESIAN_POINT('Ctrl Pts',(-1.11366113367805,-0.872999428421004,
-7.68613341355709E-16));
#7999=CARTESIAN_POINT('Ctrl Pts',(-1.15078992234189,-0.831604028494677,
-1.89431803576667E-15));
#8000=CARTESIAN_POINT('Ctrl Pts',(-1.1663202195496,-0.814289085373092,-2.36517984142906E-15));
#8001=CARTESIAN_POINT('Ctrl Pts',(-1.18144756318774,-0.796563309565334,
-2.96565948945709E-15));
#8002=CARTESIAN_POINT('Ctrl Pts',(-1.19616365544476,-0.778446114115039,
-2.76167977375508E-15));
#8003=CARTESIAN_POINT('Ctrl Pts',(-1.20483314424882,-0.767772980216839,
-2.64151201246017E-15));
#8004=CARTESIAN_POINT('Ctrl Pts',(-1.21335930009043,-0.756964325554185,
-1.86449801195046E-15));
#8005=CARTESIAN_POINT('Ctrl Pts',(-1.22172559193317,-0.746044338928061,
-1.72084568816899E-15));
#8006=CARTESIAN_POINT('Ctrl Pts',(-1.23769793947646,-0.725196653377617,
-1.44659457621046E-15));
#8007=CARTESIAN_POINT('Ctrl Pts',(-1.25310066142752,-0.70392782386896,-1.09877265170518E-15));
#8008=CARTESIAN_POINT('Ctrl Pts',(-1.26792826560863,-0.68227084872173,-1.16573417585641E-15));
#8009=CARTESIAN_POINT('Ctrl Pts',(-1.30064000206196,-0.634492579573223,
-1.313460518143E-15));
#8010=CARTESIAN_POINT('Ctrl Pts',(-1.33055288609126,-0.584830241555012,
-1.18464778661716E-15));
#8011=CARTESIAN_POINT('Ctrl Pts',(-1.35757841478232,-0.533616942208867,
-4.44089209850063E-16));
#8012=CARTESIAN_POINT('Ctrl Pts',(-1.38506646201561,-0.481527171551913,
3.09143386259586E-16));
#8013=CARTESIAN_POINT('Ctrl Pts',(-1.40956822217026,-0.427832070929981,
-9.2928198748492E-16));
#8014=CARTESIAN_POINT('Ctrl Pts',(-1.43095548368543,-0.372841920597751,
-1.0547118733939E-15));
#8015=CARTESIAN_POINT('Ctrl Pts',(-1.44153762134738,-0.345633512431298,
-1.11677294272112E-15));
#8016=CARTESIAN_POINT('Ctrl Pts',(-1.45135667973785,-0.318107521778687,
-1.09151072745545E-15));
#8017=CARTESIAN_POINT('Ctrl Pts',(-1.46039315561881,-0.290298981848618,
-6.66133814775094E-16));
#8018=CARTESIAN_POINT('Ctrl Pts',(-1.46494353283797,-0.276295807573305,
-4.5083568064057E-16));
#8019=CARTESIAN_POINT('Ctrl Pts',(-1.46929683648255,-0.26221562433059,-2.38820861466436E-15));
#8020=CARTESIAN_POINT('Ctrl Pts',(-1.473441618016,-0.248093948282024,-2.15105711021124E-15));
#8021=CARTESIAN_POINT('Ctrl Pts',(-1.4905537552228,-0.189791223233013,-1.04000775610132E-15));
#8022=CARTESIAN_POINT('Ctrl Pts',(-1.50414431451018,-0.130700983448934,
-7.32518070969078E-16));
#8023=CARTESIAN_POINT('Ctrl Pts',(-1.51411149444636,-0.0711710784181553,
-1.47104550762833E-15));
#8024=CARTESIAN_POINT('Ctrl Pts',(-1.5240471929564,-0.0118291991198427,
-2.6702633386109E-15));
#8025=CARTESIAN_POINT('Ctrl Pts',(-1.53038298344941,0.0479506119131717,
6.12492081269896E-16));
#8026=CARTESIAN_POINT('Ctrl Pts',(-1.53297599397982,0.107852419831135,1.01307850997046E-15));
#8027=CARTESIAN_POINT('Ctrl Pts',(-1.5343216654729,0.13893912555559,8.07247865597284E-16));
#8028=CARTESIAN_POINT('Ctrl Pts',(-1.53465858251287,0.170059062380459,6.33636663361729E-16));
#8029=CARTESIAN_POINT('Ctrl Pts',(-1.53396143973122,0.201169701697847,-2.91433543964104E-16));
#8030=CARTESIAN_POINT('Ctrl Pts',(-1.53315235769005,0.237275733666988,-1.31380156557419E-15));
#8031=CARTESIAN_POINT('Ctrl Pts',(-1.53095064843268,0.273369292680589,-3.47125944024131E-16));
#8032=CARTESIAN_POINT('Ctrl Pts',(-1.52739541139815,0.309398947352701,-1.02695629777827E-15));
#8033=CARTESIAN_POINT('Ctrl Pts',(-1.52629773176855,0.320523105210736,-1.40527035743221E-15));
#8034=CARTESIAN_POINT('Ctrl Pts',(-1.52507166732445,0.331633629961292,-1.02948525143009E-16));
#8035=CARTESIAN_POINT('Ctrl Pts',(-1.5237196856603,0.342722587468097,-8.32667268468867E-17));
#8036=CARTESIAN_POINT('Ctrl Pts',(-1.516518466799,0.401787005328014,-1.28384931635538E-16));
#8037=CARTESIAN_POINT('Ctrl Pts',(-1.50574358938221,0.46029506897729,-2.5884345523775E-15));
#8038=CARTESIAN_POINT('Ctrl Pts',(-1.49164313082402,0.518014064605472,-1.62370117351429E-15));
#8039=CARTESIAN_POINT('Ctrl Pts',(-1.47706888159878,0.577672480950095,-6.26551709089525E-16));
#8040=CARTESIAN_POINT('Ctrl Pts',(-1.45894176921365,0.636488725124688,7.13174734340251E-16));
#8041=CARTESIAN_POINT('Ctrl Pts',(-1.43747991265361,0.694213509478351,-4.16333634234434E-16));
#8042=CARTESIAN_POINT('Ctrl Pts',(-1.42099781437687,0.738544509737268,-1.28376408616919E-15));
#8043=CARTESIAN_POINT('Ctrl Pts',(-1.40254775675702,0.782232068197874,-9.02083324469551E-16));
#8044=CARTESIAN_POINT('Ctrl Pts',(-1.38220782814776,0.825161373923281,-6.66133814775094E-16));
#8045=CARTESIAN_POINT('Ctrl Pts',(-1.37469143189959,0.841025425301725,-6.32268855604997E-16));
#8046=CARTESIAN_POINT('Ctrl Pts',(-1.36691678867014,0.856785892169704,-1.94116254897675E-15));
#8047=CARTESIAN_POINT('Ctrl Pts',(-1.35888726366717,0.872436807123193,-1.72084568816899E-15));
#8048=CARTESIAN_POINT('Ctrl Pts',(-1.35063706597361,0.888517850821735,-1.41388399025223E-15));
#8049=CARTESIAN_POINT('Ctrl Pts',(-1.34211487275061,0.904488002686463,-1.61566361807131E-15));
#8050=CARTESIAN_POINT('Ctrl Pts',(-1.33334349594405,0.920306971938382,-1.58206781009085E-15));
#8051=CARTESIAN_POINT('Ctrl Pts',(-1.30214685892829,0.976569364103196,-1.46257958721175E-15));
#8052=CARTESIAN_POINT('Ctrl Pts',(-1.26776287350155,1.03100157507453,4.98596072913018E-16));
#8053=CARTESIAN_POINT('Ctrl Pts',(-1.23041822401205,1.08333236977297,2.77555756156289E-17));
#8054=CARTESIAN_POINT('Ctrl Pts',(-1.19893362730352,1.12745151372103,-3.6920150857429E-16));
#8055=CARTESIAN_POINT('Ctrl Pts',(-1.16534352389359,1.17007731567397,-1.15789935301514E-15));
#8056=CARTESIAN_POINT('Ctrl Pts',(-1.12975612292984,1.2110393106172,-1.94289029309402E-16));
#8057=CARTESIAN_POINT('Ctrl Pts',(-1.11980830251754,1.2224895024938,8.16785287875133E-19));
#8058=CARTESIAN_POINT('Ctrl Pts',(-1.10970427564496,1.23380962006102,-8.83756491716252E-16));
#8059=CARTESIAN_POINT('Ctrl Pts',(-1.09944608615852,1.24499576190878,-3.05311331771918E-16));
#8060=CARTESIAN_POINT('Ctrl Pts',(-1.09148793970747,1.25367379960387,2.16835242351985E-16));
#8061=CARTESIAN_POINT('Ctrl Pts',(-1.08343792396404,1.2622701055878,-4.67419621806966E-16));
#8062=CARTESIAN_POINT('Ctrl Pts',(-1.07530384816136,1.27077601604308,-2.22044604925031E-16));
#8063=CARTESIAN_POINT('Ctrl Pts',(-1.02993327554411,1.3182206228244,5.7724852838323E-16));
#8064=CARTESIAN_POINT('Ctrl Pts',(-0.98189595159246,1.36291522819749,-1.37872740780286E-15));
#8065=CARTESIAN_POINT('Ctrl Pts',(-0.931398621857827,1.40457604009645,-6.10622663543836E-16));
#8066=CARTESIAN_POINT('Ctrl Pts',(-0.881340571334673,1.44587444216707,1.50800292823326E-16));
#8067=CARTESIAN_POINT('Ctrl Pts',(-0.828864591896417,1.48419258027966,-3.05515458637289E-15));
#8068=CARTESIAN_POINT('Ctrl Pts',(-0.774129732122116,1.51922639018999,-1.52655665885959E-15));
#8069=CARTESIAN_POINT('Ctrl Pts',(-0.764997683666341,1.52507148508949,-1.24297269028027E-15));
#8070=CARTESIAN_POINT('Ctrl Pts',(-0.75580267106898,1.53082507493498,-1.52747238928381E-15));
#8071=CARTESIAN_POINT('Ctrl Pts',(-0.746545333137423,1.53648564199954,-3.88578058618805E-16));
#8072=CARTESIAN_POINT('Ctrl Pts',(0.993445330382434,-1.39216647130147,-0.198796524485181));
#8073=CARTESIAN_POINT('Ctrl Pts',(1.45224744664474,-1.06478123128123,-0.167326491865807));
#8074=CARTESIAN_POINT('Ctrl Pts',(2.01346727495692,0.0729463614329333,-0.104395023997457));
#8075=CARTESIAN_POINT('Ctrl Pts',(1.04452544803256,1.72489834357427,-0.0100021208801329));
#8076=CARTESIAN_POINT('Ctrl Pts',(-0.865118107719488,1.81944815671647,0.0843821848667926));
#8077=CARTESIAN_POINT('Ctrl Pts',(-1.99580016919685,0.279114534669996,0.178766490613719));
#8078=CARTESIAN_POINT('Ctrl Pts',(-1.33062056689224,-1.51369898506524,0.273150796360644));
#8079=CARTESIAN_POINT('Ctrl Pts',(0.532139236212413,-1.94360970629842,0.367535102107569));
#8080=CARTESIAN_POINT('Ctrl Pts',(1.91595060805295,-0.624764979528343,0.461919407854496));
#8081=CARTESIAN_POINT('Ctrl Pts',(1.57557243209307,1.25651211697159,0.556303713601421));
#8082=CARTESIAN_POINT('Ctrl Pts',(-0.18272721901878,2.00691771985262,0.650688019348347));
#8083=CARTESIAN_POINT('Ctrl Pts',(-1.77657640637496,0.951289839344929,0.745072325095271));
#8084=CARTESIAN_POINT('Ctrl Pts',(-1.77163592240772,-0.960459485878452,
0.839456630842199));
#8085=CARTESIAN_POINT('Ctrl Pts',(-0.172344824174458,-2.00784825297573,
0.933840936589122));
#8086=CARTESIAN_POINT('Ctrl Pts',(1.58204326623752,-1.24832180902719,1.02822524233605));
#8087=CARTESIAN_POINT('Ctrl Pts',(1.91270394017647,0.634610748931089,1.12260954808298));
#8088=CARTESIAN_POINT('Ctrl Pts',(0.522064739489251,1.94643602090733,1.2169938538299));
#8089=CARTESIAN_POINT('Ctrl Pts',(-1.33839596074812,1.50660635374839,1.31137815957683));
#8090=CARTESIAN_POINT('Ctrl Pts',(-1.9943941749754,-0.289064038131091,1.40576246532376));
#8091=CARTESIAN_POINT('Ctrl Pts',(-0.855577327983737,-1.82459674855572,
1.50014677107068));
#8092=CARTESIAN_POINT('Ctrl Pts',(1.05319913699118,-1.71812039355476,1.59453107681761));
#8093=CARTESIAN_POINT('Ctrl Pts',(2.01417019051478,-0.0654559897729185,
1.68891538256453));
#8094=CARTESIAN_POINT('Ctrl Pts',(1.16252919819725,1.64611417447018,1.78329968831146));
#8095=CARTESIAN_POINT('Ctrl Pts',(-0.735306610103401,1.87629694805414,1.87768399405838));
#8096=CARTESIAN_POINT('Ctrl Pts',(-1.97141799434173,0.417943928532112,1.97206829980531));
#8097=CARTESIAN_POINT('Ctrl Pts',(-1.43339131998399,-1.41652933494684,2.06645260555223));
#8098=CARTESIAN_POINT('Ctrl Pts',(0.394587103969732,-1.97622545662158,2.16083691129916));
#8099=CARTESIAN_POINT('Ctrl Pts',(1.86746478339235,-0.757457139826309,2.25522121704609));
#8100=CARTESIAN_POINT('Ctrl Pts',(1.65975501098531,1.14296952681729,2.34960552279301));
#8101=CARTESIAN_POINT('Ctrl Pts',(-0.0416179720839357,2.01480370776058,
2.44398982853993));
#8102=CARTESIAN_POINT('Ctrl Pts',(-1.70553769649486,1.07345572889199,2.53837413428687));
#8103=CARTESIAN_POINT('Ctrl Pts',(-1.83459300117589,-0.833927188731956,
2.63275844003379));
#8104=CARTESIAN_POINT('Ctrl Pts',(-0.312643154862414,-1.99083406990042,
2.72714274578071));
#8105=CARTESIAN_POINT('Ctrl Pts',(1.49066362390716,-1.35612978599523,2.82152705152764));
#8106=CARTESIAN_POINT('Ctrl Pts',(1.95247759205483,0.498996281183202,2.91591135727456));
#8107=CARTESIAN_POINT('Ctrl Pts',(0.657198537587743,1.9050606600091,3.0102956630215));
#8108=CARTESIAN_POINT('Ctrl Pts',(-1.22951315076462,1.5967039325468,3.10467996876841));
#8109=CARTESIAN_POINT('Ctrl Pts',(-2.0097491554954,-0.148574453055689,3.19906427451535));
#8110=CARTESIAN_POINT('Ctrl Pts',(-0.981351743535662,-1.76014624153099,
3.29344858026226));
#8111=CARTESIAN_POINT('Ctrl Pts',(0.930193474225359,-1.78770974619056,3.3878328860092));
#8112=CARTESIAN_POINT('Ctrl Pts',(2.0046297439011,-0.206459744217345,3.48221719175612));
#8113=CARTESIAN_POINT('Ctrl Pts',(1.27503970860364,1.5605895609024,3.57660149750304));
#8114=CARTESIAN_POINT('Ctrl Pts',(-0.601996722321556,1.92321761182553,3.67098580324997));
#8115=CARTESIAN_POINT('Ctrl Pts',(-1.93727828510637,0.555084572084459,3.76537010899689));
#8116=CARTESIAN_POINT('Ctrl Pts',(-1.52914513651331,-1.31258568771001,3.85975441474383));
#8117=CARTESIAN_POINT('Ctrl Pts',(0.255111487644501,-1.9990208015502,3.95413872049074));
#8118=CARTESIAN_POINT('Ctrl Pts',(1.80978564859574,-0.886477265476602,4.04852302623767));
#8119=CARTESIAN_POINT('Ctrl Pts',(1.73577953761973,1.02383369393503,4.1429073319846));
#8120=CARTESIAN_POINT('Ctrl Pts',(0.0996934689531183,2.01276606903392,4.23729163773152));
#8121=CARTESIAN_POINT('Ctrl Pts',(-1.62610973620759,1.1903500163963,4.33167594347845));
#8122=CARTESIAN_POINT('Ctrl Pts',(-1.88852812046539,-0.703297642606548,
4.42606024922538));
#8123=CARTESIAN_POINT('Ctrl Pts',(-0.45140352546393,-1.96402670430346,4.5204445549723));
#8124=CARTESIAN_POINT('Ctrl Pts',(1.39195261233386,-1.45726934984146,4.61482886071923));
#8125=CARTESIAN_POINT('Ctrl Pts',(1.98264893371114,0.360928305159485,4.70921316646615));
#8126=CARTESIAN_POINT('Ctrl Pts',(0.789100138196465,1.8543157821788,4.80359747221308));
#8127=CARTESIAN_POINT('Ctrl Pts',(-1.1145834876982,1.67894897510415,4.89798177796));
#8128=CARTESIAN_POINT('Ctrl Pts',(-2.01522007683398,-0.00735424236076328,
4.99236608370693));
#8129=CARTESIAN_POINT('Ctrl Pts',(-1.10229979727379,-1.68703920103769,5.08675038945385));
#8130=CARTESIAN_POINT('Ctrl Pts',(0.802613049915853,-1.8485070059658,5.18113469520079));
#8131=CARTESIAN_POINT('Ctrl Pts',(1.98523041358707,-0.346448189900541,5.2755190009477));
#8132=CARTESIAN_POINT('Ctrl Pts',(1.38127946790861,1.46739002464785,5.36990330669464));
#8133=CARTESIAN_POINT('Ctrl Pts',(-0.465726131974941,1.96067946021252,5.46428761244155));
#8134=CARTESIAN_POINT('Ctrl Pts',(-1.89361099983627,0.689495864182337,5.55867191818849));
#8135=CARTESIAN_POINT('Ctrl Pts',(-1.61737836162868,-1.20218778503015,5.6530562239354));
#8136=CARTESIAN_POINT('Ctrl Pts',(0.114380917309485,-2.01198269156394,5.74744052968234));
#8137=CARTESIAN_POINT('Ctrl Pts',(1.74320644116969,-1.01114171560858,5.84182483542925));
#8138=CARTESIAN_POINT('Ctrl Pts',(1.80326630572656,0.899670337824012,5.93620914117619));
#8139=CARTESIAN_POINT('Ctrl Pts',(0.240516672199542,2.00081475934751,6.03059344692311));
#8140=CARTESIAN_POINT('Ctrl Pts',(-1.53868838529779,1.30141816562462,6.12497775267004));
#8141=CARTESIAN_POINT('Ctrl Pts',(-1.93316787609034,-0.569262659056326,
6.21936205841696));
#8142=CARTESIAN_POINT('Ctrl Pts',(-0.587958060108795,-1.92745847599559,
6.31374636416389));
#8143=CARTESIAN_POINT('Ctrl Pts',(1.28642289607729,-1.5514354136967,6.40813066991081));
#8144=CARTESIAN_POINT('Ctrl Pts',(2.00301810604117,0.221453619752493,6.50251497565774));
#8145=CARTESIAN_POINT('Ctrl Pts',(0.917218545591866,1.79374777349143,6.59689928140466));
#8146=CARTESIAN_POINT('Ctrl Pts',(-0.994357215842109,1.75429798909866,6.69128358715159));
#8147=CARTESIAN_POINT('Ctrl Pts',(-2.01046165517952,0.131074529887547,6.78567042953023));
#8148=CARTESIAN_POINT('Ctrl Pts',(-1.48244620740138,-1.02224374889723,6.84859583665991));
#8149=CARTESIAN_POINT('Ctrl Pts',(-1.03343210425486,-1.36274693512055,6.88005980854061));
#8150=CARTESIAN_POINT('Ctrl Pts',(0.926331970733012,-1.29811703926643,-0.132089456432433));
#8151=CARTESIAN_POINT('Ctrl Pts',(1.35413917414512,-0.992848691525437,-0.100619423813059));
#8152=CARTESIAN_POINT('Ctrl Pts',(1.87744514144454,0.0680183847841591,-0.0376879559447101));
#8153=CARTESIAN_POINT('Ctrl Pts',(0.973961311373108,1.60837082127324,0.0567049471726145));
#8154=CARTESIAN_POINT('Ctrl Pts',(-0.806674043484716,1.69653321135336,0.15108925291954));
#8155=CARTESIAN_POINT('Ctrl Pts',(-1.86097155764947,0.260258626271408,0.245473558666466));
#8156=CARTESIAN_POINT('Ctrl Pts',(-1.24072894031588,-1.41143928211153,0.33985786441339));
#8157=CARTESIAN_POINT('Ctrl Pts',(0.496189948565409,-1.81230688243118,0.434242170160317));
#8158=CARTESIAN_POINT('Ctrl Pts',(1.78651632687384,-0.582558251603697,0.528626475907242));
#8159=CARTESIAN_POINT('Ctrl Pts',(1.46913279615649,1.17162697328914,0.623010781654168));
#8160=CARTESIAN_POINT('Ctrl Pts',(-0.170382868310501,1.87133804918526,0.717395087401093));
#8161=CARTESIAN_POINT('Ctrl Pts',(-1.65655771218086,0.887024343130625,0.811779393148019));
#8162=CARTESIAN_POINT('Ctrl Pts',(-1.65195098837856,-0.895574523482337,
0.906163698894944));
#8163=CARTESIAN_POINT('Ctrl Pts',(-0.160701868276632,-1.87220571905636,
1.00054800464187));
#8164=CARTESIAN_POINT('Ctrl Pts',(1.47516648554233,-1.16398997116428,1.09493231038879));
#8165=CARTESIAN_POINT('Ctrl Pts',(1.78348899143789,0.591738878554484,1.18931661613572));
#8166=CARTESIAN_POINT('Ctrl Pts',(0.486796046235497,1.81494226205554,1.28370092188264));
#8167=CARTESIAN_POINT('Ctrl Pts',(-1.24797905835808,1.40482580178756,1.37808522762957));
#8168=CARTESIAN_POINT('Ctrl Pts',(-1.85966054700985,-0.269535979405069,
1.4724695333765));
#8169=CARTESIAN_POINT('Ctrl Pts',(-0.797777802267743,-1.70133398405729,
1.56685383912342));
#8170=CARTESIAN_POINT('Ctrl Pts',(0.982049039143188,-1.60205076358401,1.66123814487035));
#8171=CARTESIAN_POINT('Ctrl Pts',(1.87810057072086,-0.0610340339304603,
1.75562245061727));
#8172=CARTESIAN_POINT('Ctrl Pts',(1.08399318036572,1.53490900873377,1.8500067563642));
#8173=CARTESIAN_POINT('Ctrl Pts',(-0.685632113211391,1.74954151619218,1.94439106211112));
#8174=CARTESIAN_POINT('Ctrl Pts',(-1.83823654909533,0.389709238276857,2.03877536785805));
#8175=CARTESIAN_POINT('Ctrl Pts',(-1.33655689514511,-1.32083404120213,2.13315967360497));
#8176=CARTESIAN_POINT('Ctrl Pts',(0.367930311278841,-1.8427192376457,2.2275439793519));
#8177=CARTESIAN_POINT('Ctrl Pts',(1.74130601873017,-0.706286238026784,2.32192828509883));
#8178=CARTESIAN_POINT('Ctrl Pts',(1.54762832260548,1.06575488543175,2.41631259084575));
#8179=CARTESIAN_POINT('Ctrl Pts',(-0.0388064213695487,1.87869128996917,
2.51069689659268));
#8180=CARTESIAN_POINT('Ctrl Pts',(-1.59031810532073,1.00093717331819,2.6050812023396));
#8181=CARTESIAN_POINT('Ctrl Pts',(-1.71065492815597,-0.777590263460737,
2.69946550808653));
#8182=CARTESIAN_POINT('Ctrl Pts',(-0.291522181364917,-1.85634094899147,
2.79384981383345));
#8183=CARTESIAN_POINT('Ctrl Pts',(1.38996010168205,-1.26451485432732,2.88823411958038));
#8184=CARTESIAN_POINT('Ctrl Pts',(1.82057568780754,0.465286004574547,2.9826184253273));
#8185=CARTESIAN_POINT('Ctrl Pts',(0.612800722765632,1.77636206198968,3.07700273107423));
#8186=CARTESIAN_POINT('Ctrl Pts',(-1.14645195377939,1.48883673341525,3.17138703682116));
#8187=CARTESIAN_POINT('Ctrl Pts',(-1.87397820388604,-0.138537332342868,
3.26577134256808));
#8188=CARTESIAN_POINT('Ctrl Pts',(-0.915055380271112,-1.64123750631354,
3.36015564831501));
#8189=CARTESIAN_POINT('Ctrl Pts',(0.867353167597517,-1.66693892622134,3.45453995406193));
#8190=CARTESIAN_POINT('Ctrl Pts',(1.86920464012152,-0.192512115049408,3.54892425980886));
#8191=CARTESIAN_POINT('Ctrl Pts',(1.18890291182804,1.45516211032929,3.64330856555578));
#8192=CARTESIAN_POINT('Ctrl Pts',(-0.561328130606112,1.79329239971861,3.73769287130272));
#8193=CARTESIAN_POINT('Ctrl Pts',(-1.80640318779295,0.517585185472195,3.83207717704963));
#8194=CARTESIAN_POINT('Ctrl Pts',(-1.42584195075725,-1.22391242846177,3.92646148279657));
#8195=CARTESIAN_POINT('Ctrl Pts',(0.237877133123564,-1.86397461642245,4.02084578854348));
#8196=CARTESIAN_POINT('Ctrl Pts',(1.68752346525464,-0.826590258391798,4.11523009429042));
#8197=CARTESIAN_POINT('Ctrl Pts',(1.61851692354558,0.954667412891863,4.20961440003733));
#8198=CARTESIAN_POINT('Ctrl Pts',(0.0929585602148776,1.87679130630668,4.30399870578427));
#8199=CARTESIAN_POINT('Ctrl Pts',(-1.51625599366343,1.10993453069628,4.39838301153119));
#8200=CARTESIAN_POINT('Ctrl Pts',(-1.76094639746502,-0.655785548900625,
4.49276731727812));
#8201=CARTESIAN_POINT('Ctrl Pts',(-0.420908433056757,-1.83134458628871,
4.58715162302504));
#8202=CARTESIAN_POINT('Ctrl Pts',(1.29791762779116,-1.35882181680575,4.68153592877197));
#8203=CARTESIAN_POINT('Ctrl Pts',(1.84870876923778,0.336545371936081,4.77592023451889));
#8204=CARTESIAN_POINT('Ctrl Pts',(0.735791556682662,1.7290453136518,4.87030454026581));
#8205=CARTESIAN_POINT('Ctrl Pts',(-1.03928649834056,1.56552561605949,4.96468884601275));
#8206=CARTESIAN_POINT('Ctrl Pts',(-1.8790795307435,-0.00685741792825145,
5.05907315175966));
#8207=CARTESIAN_POINT('Ctrl Pts',(-1.02783264697026,-1.57306929733063,5.1534574575066));
#8208=CARTESIAN_POINT('Ctrl Pts',(0.748391587867626,-1.72362895610057,5.24784176325352));
#8209=CARTESIAN_POINT('Ctrl Pts',(1.8511158542255,-0.323043477776379,5.34222606900045));
#8210=CARTESIAN_POINT('Ctrl Pts',(1.28796552010391,1.36825877760454,5.43661037474737));
#8211=CARTESIAN_POINT('Ctrl Pts',(-0.434263459155965,1.82822346918195,5.53099468049429));
#8212=CARTESIAN_POINT('Ctrl Pts',(-1.76568589698316,0.642916165738485,5.62537898624123));
#8213=CARTESIAN_POINT('Ctrl Pts',(-1.50811447729253,-1.12097258504345,5.71976329198815));
#8214=CARTESIAN_POINT('Ctrl Pts',(0.106653780842439,-1.87606085081667,5.81414759773507));
#8215=CARTESIAN_POINT('Ctrl Pts',(1.62544209395152,-0.942832855985621,5.908531903482));
#8216=CARTESIAN_POINT('Ctrl Pts',(1.68144454420765,0.838892057327132,6.00291620922892));
#8217=CARTESIAN_POINT('Ctrl Pts',(0.224268287482887,1.86564738130541,6.09730051497587));
#8218=CARTESIAN_POINT('Ctrl Pts',(-1.43474049422346,1.21349934137462,6.19168482072277));
#8219=CARTESIAN_POINT('Ctrl Pts',(-1.80257046225899,-0.530805455218523,
6.28606912646971));
#8220=CARTESIAN_POINT('Ctrl Pts',(-0.548237866616442,-1.7972467673563,6.38045343221663));
#8221=CARTESIAN_POINT('Ctrl Pts',(1.19951709477623,-1.44662638223021,6.47483773796356));
#8222=CARTESIAN_POINT('Ctrl Pts',(1.86770187833963,0.206493061809774,6.56922204371047));
#8223=CARTESIAN_POINT('Ctrl Pts',(0.855254775422712,1.67256904753542,6.66360634945741));
#8224=CARTESIAN_POINT('Ctrl Pts',(-0.927182252705367,1.6357843394051,6.75799065520433));
#8225=CARTESIAN_POINT('Ctrl Pts',(-1.87464256982179,0.122219636924447,6.85237749758299));
#8226=CARTESIAN_POINT('Ctrl Pts',(-1.38229782234636,-0.953184878448155,
6.91530290471266));
#8227=CARTESIAN_POINT('Ctrl Pts',(-0.963617391391471,-1.27068497421457,
6.94676687659335));
#8228=CARTESIAN_POINT('Ctrl Pts',(0.859218611083588,-1.20406760723138,-0.0653823883796859));
#8229=CARTESIAN_POINT('Ctrl Pts',(1.25603090164551,-0.920916151769643,-0.0339123557603118));
#8230=CARTESIAN_POINT('Ctrl Pts',(1.74142300793214,0.0630904081353831,0.0290191121080374));
#8231=CARTESIAN_POINT('Ctrl Pts',(0.903397174713665,1.49184329897221,0.123412015225362));
#8232=CARTESIAN_POINT('Ctrl Pts',(-0.748229979249945,1.57361826599023,0.217796320972287));
#8233=CARTESIAN_POINT('Ctrl Pts',(-1.72614294610208,0.24140271787282,0.312180626719213));
#8234=CARTESIAN_POINT('Ctrl Pts',(-1.15083731373951,-1.30917957915784,0.406564932466139));
#8235=CARTESIAN_POINT('Ctrl Pts',(0.460240660918409,-1.68100405856396,0.500949238213064));
#8236=CARTESIAN_POINT('Ctrl Pts',(1.65708204569473,-0.540351523679055,0.59533354395999));
#8237=CARTESIAN_POINT('Ctrl Pts',(1.36269316021993,1.08674182960668,0.689717849706915));
#8238=CARTESIAN_POINT('Ctrl Pts',(-0.158038517602226,1.7357583785179,0.784102155453842));
#8239=CARTESIAN_POINT('Ctrl Pts',(-1.53653901798676,0.822758846916326,0.878486461200766));
#8240=CARTESIAN_POINT('Ctrl Pts',(-1.53226605434941,-0.830689561086225,
0.972870766947694));
#8241=CARTESIAN_POINT('Ctrl Pts',(-0.149058912378804,-1.73656318513701,
1.06725507269462));
#8242=CARTESIAN_POINT('Ctrl Pts',(1.36828970484713,-1.07965813330138,1.16163937844154));
#8243=CARTESIAN_POINT('Ctrl Pts',(1.65427404269931,0.54886700817788,1.25602368418847));
#8244=CARTESIAN_POINT('Ctrl Pts',(0.451527352981743,1.68344850320373,1.3504079899354));
#8245=CARTESIAN_POINT('Ctrl Pts',(-1.15756215596805,1.30304524982673,1.44479229568232));
#8246=CARTESIAN_POINT('Ctrl Pts',(-1.72492691904432,-0.250007920679045,
1.53917660142925));
#8247=CARTESIAN_POINT('Ctrl Pts',(-0.739978276551748,-1.57807121955886,
1.63356090717617));
#8248=CARTESIAN_POINT('Ctrl Pts',(0.910898941295185,-1.48598113361326,1.7279452129231));
#8249=CARTESIAN_POINT('Ctrl Pts',(1.74203095092696,-0.0566120780880063,
1.82232951867002));
#8250=CARTESIAN_POINT('Ctrl Pts',(1.00545716253417,1.42370384299737,1.91671382441695));
#8251=CARTESIAN_POINT('Ctrl Pts',(-0.635957616319379,1.6227860843302,2.01109813016387));
#8252=CARTESIAN_POINT('Ctrl Pts',(-1.70505510384895,0.361474548021605,2.1054824359108));
#8253=CARTESIAN_POINT('Ctrl Pts',(-1.23972247030623,-1.22513874745744,2.19986674165772));
#8254=CARTESIAN_POINT('Ctrl Pts',(0.341273518587947,-1.70921301866982,2.29425104740465));
#8255=CARTESIAN_POINT('Ctrl Pts',(1.61514725406801,-0.655115336227261,2.38863535315157));
#8256=CARTESIAN_POINT('Ctrl Pts',(1.43550163422564,0.988540244046207,2.4830196588985));
#8257=CARTESIAN_POINT('Ctrl Pts',(-0.0359948706551594,1.74257887217777,
2.57740396464543));
#8258=CARTESIAN_POINT('Ctrl Pts',(-1.47509851414659,0.928418617744392,2.67178827039235));
#8259=CARTESIAN_POINT('Ctrl Pts',(-1.58671685513604,-0.721253338189517,
2.76617257613928));
#8260=CARTESIAN_POINT('Ctrl Pts',(-0.27040120786742,-1.72184782808252,2.8605568818862));
#8261=CARTESIAN_POINT('Ctrl Pts',(1.28925657945695,-1.1728999226594,2.95494118763313));
#8262=CARTESIAN_POINT('Ctrl Pts',(1.68867378356024,0.431575727965893,3.04932549338005));
#8263=CARTESIAN_POINT('Ctrl Pts',(0.56840290794352,1.64766346397025,3.14370979912698));
#8264=CARTESIAN_POINT('Ctrl Pts',(-1.06339075679415,1.38096953428369,3.2380941048739));
#8265=CARTESIAN_POINT('Ctrl Pts',(-1.73820725227668,-0.128500211630046,
3.33247841062083));
#8266=CARTESIAN_POINT('Ctrl Pts',(-0.848759017006559,-1.52232877109609,
3.42686271636775));
#8267=CARTESIAN_POINT('Ctrl Pts',(0.804512860969673,-1.54616810625213,3.52124702211469));
#8268=CARTESIAN_POINT('Ctrl Pts',(1.73377953634196,-0.17856448588147,3.61563132786161));
#8269=CARTESIAN_POINT('Ctrl Pts',(1.10276611505244,1.34973465975617,3.71001563360853));
#8270=CARTESIAN_POINT('Ctrl Pts',(-0.520659538890669,1.6633671876117,3.80439993935546));
#8271=CARTESIAN_POINT('Ctrl Pts',(-1.67552809047953,0.480085798859931,3.89878424510239));
#8272=CARTESIAN_POINT('Ctrl Pts',(-1.32253876500119,-1.13523916921351,3.99316855084931));
#8273=CARTESIAN_POINT('Ctrl Pts',(0.220642778602628,-1.7289284312947,4.08755285659624));
#8274=CARTESIAN_POINT('Ctrl Pts',(1.56526128191355,-0.766703251306995,4.18193716234316));
#8275=CARTESIAN_POINT('Ctrl Pts',(1.50125430947145,0.88550113184869,4.27632146809009));
#8276=CARTESIAN_POINT('Ctrl Pts',(0.0862236514766394,1.74081654357945,4.37070577383701));
#8277=CARTESIAN_POINT('Ctrl Pts',(-1.40640225111927,1.02951904499627,4.46509007958394));
#8278=CARTESIAN_POINT('Ctrl Pts',(-1.63336467446466,-0.608273455194703,
4.55947438533086));
#8279=CARTESIAN_POINT('Ctrl Pts',(-0.390413340649585,-1.69866246827398,
4.65385869107779));
#8280=CARTESIAN_POINT('Ctrl Pts',(1.20388264324848,-1.26037428377003,4.74824299682472));
#8281=CARTESIAN_POINT('Ctrl Pts',(1.71476860476443,0.312162438712672,4.84262730257164));
#8282=CARTESIAN_POINT('Ctrl Pts',(0.682482975168861,1.60377484512479,4.93701160831856));
#8283=CARTESIAN_POINT('Ctrl Pts',(-0.963989508982937,1.45210225701483,5.03139591406549));
#8284=CARTESIAN_POINT('Ctrl Pts',(-1.74293898465302,-0.00636059349573666,
5.12578021981242));
#8285=CARTESIAN_POINT('Ctrl Pts',(-0.953365496666722,-1.45909939362356,
5.22016452555934));
#8286=CARTESIAN_POINT('Ctrl Pts',(0.694170125819397,-1.59875090623536,5.31454883130627));
#8287=CARTESIAN_POINT('Ctrl Pts',(1.71700129486393,-0.299638765652215,5.40893313705319));
#8288=CARTESIAN_POINT('Ctrl Pts',(1.19465157229921,1.26912753056122,5.50331744280012));
#8289=CARTESIAN_POINT('Ctrl Pts',(-0.402800786336985,1.69576747815139,5.59770174854704));
#8290=CARTESIAN_POINT('Ctrl Pts',(-1.63776079413004,0.596336467294631,5.69208605429397));
#8291=CARTESIAN_POINT('Ctrl Pts',(-1.39885059295638,-1.03975738505673,5.7864703600409));
#8292=CARTESIAN_POINT('Ctrl Pts',(0.09892664437539,-1.74013901006941,5.88085466578782));
#8293=CARTESIAN_POINT('Ctrl Pts',(1.50767774673337,-0.874523996362657,5.97523897153475));
#8294=CARTESIAN_POINT('Ctrl Pts',(1.55962278268874,0.778113776830252,6.06962327728167));
#8295=CARTESIAN_POINT('Ctrl Pts',(0.208019902766231,1.73048000326329,6.1640075830286));
#8296=CARTESIAN_POINT('Ctrl Pts',(-1.33079260314915,1.12558051712463,6.25839188877553));
#8297=CARTESIAN_POINT('Ctrl Pts',(-1.67197304842765,-0.49234825138072,6.35277619452245));
#8298=CARTESIAN_POINT('Ctrl Pts',(-0.508517673124086,-1.667035058717,6.44716050026938));
#8299=CARTESIAN_POINT('Ctrl Pts',(1.11261129347517,-1.34181735076373,6.5415448060163));
#8300=CARTESIAN_POINT('Ctrl Pts',(1.7323856506381,0.191532503867054,6.63592911176323));
#8301=CARTESIAN_POINT('Ctrl Pts',(0.793291005253558,1.55139032157942,6.73031341751015));
#8302=CARTESIAN_POINT('Ctrl Pts',(-0.860007289568625,1.51727068971153,6.82469772325708));
#8303=CARTESIAN_POINT('Ctrl Pts',(-1.73882348446406,0.113364743961346,6.91908456563572));
#8304=CARTESIAN_POINT('Ctrl Pts',(-1.28214943729133,-0.884126007999086,
6.9820099727654));
#8305=CARTESIAN_POINT('Ctrl Pts',(-0.893802678528082,-1.17862301330859,
7.0134739446461));
#8306=CARTESIAN_POINT('Ctrl Pts',(0.792105251434166,-1.11001817519634,0.00132467967306148));
#8307=CARTESIAN_POINT('Ctrl Pts',(1.1579226291459,-0.84898361201385,0.0327947122924356));
#8308=CARTESIAN_POINT('Ctrl Pts',(1.60540087441976,0.058162431486608,0.0957261801607845));
#8309=CARTESIAN_POINT('Ctrl Pts',(0.83283303805422,1.37531577667117,0.19011908327811));
#8310=CARTESIAN_POINT('Ctrl Pts',(-0.689785915015175,1.45070332062712,0.284503389025035));
#8311=CARTESIAN_POINT('Ctrl Pts',(-1.59131433455471,0.222546809474231,0.378887694771962));
#8312=CARTESIAN_POINT('Ctrl Pts',(-1.06094568716315,-1.20691987620413,0.473272000518886));
#8313=CARTESIAN_POINT('Ctrl Pts',(0.424291373271407,-1.54970123469673,0.567656306265813));
#8314=CARTESIAN_POINT('Ctrl Pts',(1.52764776451562,-0.498144795754411,0.662040612012736));
#8315=CARTESIAN_POINT('Ctrl Pts',(1.25625352428336,1.00185668592423,0.756424917759663));
#8316=CARTESIAN_POINT('Ctrl Pts',(-0.145694166893949,1.60017870785054,0.850809223506588));
#8317=CARTESIAN_POINT('Ctrl Pts',(-1.41652032379266,0.758493350702024,0.945193529253515));
#8318=CARTESIAN_POINT('Ctrl Pts',(-1.41258112032025,-0.765804598690109,
1.03957783500044));
#8319=CARTESIAN_POINT('Ctrl Pts',(-0.137415956480979,-1.60092065121764,
1.13396214074737));
#8320=CARTESIAN_POINT('Ctrl Pts',(1.26141292415194,-0.995326295438471,1.22834644649429));
#8321=CARTESIAN_POINT('Ctrl Pts',(1.52505909396075,0.505995137801276,1.32273075224122));
#8322=CARTESIAN_POINT('Ctrl Pts',(0.416258659727988,1.55195474435194,1.41711505798814));
#8323=CARTESIAN_POINT('Ctrl Pts',(-1.06714525357801,1.20126469786591,1.51149936373507));
#8324=CARTESIAN_POINT('Ctrl Pts',(-1.59019329107878,-0.230479861953022,
1.605883669482));
#8325=CARTESIAN_POINT('Ctrl Pts',(-0.682178750835754,-1.45480845506043,
1.70026797522892));
#8326=CARTESIAN_POINT('Ctrl Pts',(0.839748843447184,-1.3699115036425,1.79465228097585));
#8327=CARTESIAN_POINT('Ctrl Pts',(1.60596133113304,-0.0521901222455495,
1.88903658672277));
#8328=CARTESIAN_POINT('Ctrl Pts',(0.926921144702626,1.31249867726097,1.9834208924697));
#8329=CARTESIAN_POINT('Ctrl Pts',(-0.586283119427368,1.49603065246823,2.07780519821662));
#8330=CARTESIAN_POINT('Ctrl Pts',(-1.57187365860257,0.33323985776635,2.17218950396355));
#8331=CARTESIAN_POINT('Ctrl Pts',(-1.14288804546734,-1.12944345371274,2.26657380971047));
#8332=CARTESIAN_POINT('Ctrl Pts',(0.314616725897053,-1.57570679969394,2.3609581154574));
#8333=CARTESIAN_POINT('Ctrl Pts',(1.48898848940584,-0.603944434427737,2.45534242120432));
#8334=CARTESIAN_POINT('Ctrl Pts',(1.32337494584579,0.911325602660668,2.54972672695125));
#8335=CARTESIAN_POINT('Ctrl Pts',(-0.0331833199407702,1.60646645438636,
2.64411103269818));
#8336=CARTESIAN_POINT('Ctrl Pts',(-1.35987892297247,0.855900062170592,2.7384953384451));
#8337=CARTESIAN_POINT('Ctrl Pts',(-1.46277878211612,-0.664916412918296,
2.83287964419203));
#8338=CARTESIAN_POINT('Ctrl Pts',(-0.249280234369926,-1.58735470717356,
2.92726394993895));
#8339=CARTESIAN_POINT('Ctrl Pts',(1.18855305723184,-1.08128499099147,3.02164825568588));
#8340=CARTESIAN_POINT('Ctrl Pts',(1.55677187931295,0.397865451357236,3.1160325614328));
#8341=CARTESIAN_POINT('Ctrl Pts',(0.524005093121412,1.51896486595083,3.21041686717973));
#8342=CARTESIAN_POINT('Ctrl Pts',(-0.98032955980891,1.27310233515215,3.30480117292666));
#8343=CARTESIAN_POINT('Ctrl Pts',(-1.60243630066732,-0.118463090917224,
3.39918547867358));
#8344=CARTESIAN_POINT('Ctrl Pts',(-0.782462653742007,-1.40342003587865,
3.49356978442051));
#8345=CARTESIAN_POINT('Ctrl Pts',(0.74167255434183,-1.42539728628291,3.58795409016743));
#8346=CARTESIAN_POINT('Ctrl Pts',(1.59835443256238,-0.164616856713533,3.68233839591436));
#8347=CARTESIAN_POINT('Ctrl Pts',(1.01662931827683,1.24430720918307,3.77672270166128));
#8348=CARTESIAN_POINT('Ctrl Pts',(-0.479990947175226,1.53344197550478,3.87110700740821));
#8349=CARTESIAN_POINT('Ctrl Pts',(-1.54465299316611,0.442586412247669,3.96549131315514));
#8350=CARTESIAN_POINT('Ctrl Pts',(-1.21923557924511,-1.04656590996525,4.05987561890206));
#8351=CARTESIAN_POINT('Ctrl Pts',(0.203408424081691,-1.59388224616695,4.15425992464898));
#8352=CARTESIAN_POINT('Ctrl Pts',(1.44299909857244,-0.706816244222193,4.24864423039592));
#8353=CARTESIAN_POINT('Ctrl Pts',(1.3839916953973,0.816334850805521,4.34302853614283));
#8354=CARTESIAN_POINT('Ctrl Pts',(0.0794887427383994,1.60484178085219,4.43741284188977));
#8355=CARTESIAN_POINT('Ctrl Pts',(-1.29654850857511,0.949103559296265,4.53179714763668));
#8356=CARTESIAN_POINT('Ctrl Pts',(-1.50578295146431,-0.56076136148878,4.62618145338362));
#8357=CARTESIAN_POINT('Ctrl Pts',(-0.359918248242413,-1.56598035025924,
4.72056575913053));
#8358=CARTESIAN_POINT('Ctrl Pts',(1.10984765870579,-1.16192675073432,4.81495006487747));
#8359=CARTESIAN_POINT('Ctrl Pts',(1.58082844029107,0.287779505489267,4.90933437062438));
#8360=CARTESIAN_POINT('Ctrl Pts',(0.62917439365506,1.47850437659778,5.00371867637132));
#8361=CARTESIAN_POINT('Ctrl Pts',(-0.888692519625303,1.33867889797018,5.09810298211823));
#8362=CARTESIAN_POINT('Ctrl Pts',(-1.60679843856254,-0.00586376906322344,
5.19248728786518));
#8363=CARTESIAN_POINT('Ctrl Pts',(-0.878898346363189,-1.34512948991649,
5.28687159361209));
#8364=CARTESIAN_POINT('Ctrl Pts',(0.639948663771169,-1.47387285637013,5.38125589935902));
#8365=CARTESIAN_POINT('Ctrl Pts',(1.58288673550236,-0.276234053528054,5.47564020510594));
#8366=CARTESIAN_POINT('Ctrl Pts',(1.10133762449452,1.16999628351791,5.57002451085287));
#8367=CARTESIAN_POINT('Ctrl Pts',(-0.371338113518008,1.56331148712083,5.6644088165998));
#8368=CARTESIAN_POINT('Ctrl Pts',(-1.50983569127691,0.54975676885078,5.75879312234672));
#8369=CARTESIAN_POINT('Ctrl Pts',(-1.28958670862024,-0.958542185070025,
5.85317742809365));
#8370=CARTESIAN_POINT('Ctrl Pts',(0.0911995079083431,-1.60421716932215,
5.94756173384057));
#8371=CARTESIAN_POINT('Ctrl Pts',(1.38991339951521,-0.806215136739692,6.0419460395875));
#8372=CARTESIAN_POINT('Ctrl Pts',(1.43780102116983,0.717335496333373,6.13633034533442));
#8373=CARTESIAN_POINT('Ctrl Pts',(0.191771518049578,1.59531262522119,6.23071465108135));
#8374=CARTESIAN_POINT('Ctrl Pts',(-1.22684471207484,1.03766169287464,6.32509895682827));
#8375=CARTESIAN_POINT('Ctrl Pts',(-1.5413756345963,-0.453891047542918,6.4194832625752));
#8376=CARTESIAN_POINT('Ctrl Pts',(-0.468797479631732,-1.53682335007771,
6.51386756832213));
#8377=CARTESIAN_POINT('Ctrl Pts',(1.0257054921741,-1.23700831929723,6.60825187406904));
#8378=CARTESIAN_POINT('Ctrl Pts',(1.59706942293656,0.176571945924337,6.70263617981598));
#8379=CARTESIAN_POINT('Ctrl Pts',(0.731327235084403,1.43021159562341,6.79702048556289));
#8380=CARTESIAN_POINT('Ctrl Pts',(-0.792832326431882,1.39875704001798,6.89140479130984));
#8381=CARTESIAN_POINT('Ctrl Pts',(-1.60300439910634,0.104509850998243,6.98579163368847));
#8382=CARTESIAN_POINT('Ctrl Pts',(-1.1820010522363,-0.815067137550017,7.04871704081814));
#8383=CARTESIAN_POINT('Ctrl Pts',(-0.823987965664692,-1.08656105240261,
7.08018101269885));
#8384=CARTESIAN_POINT('',(-0.562200904851585,1.2460199179177,6.88180017065881));
#8385=CARTESIAN_POINT('Ctrl Pts',(-0.562671582971943,1.24691123662228,6.88122480138927));
#8386=CARTESIAN_POINT('Ctrl Pts',(-0.603396319682483,1.23447102102747,6.88122480138927));
#8387=CARTESIAN_POINT('Ctrl Pts',(-0.643403900568493,1.22005362851167,6.88122480138927));
#8388=CARTESIAN_POINT('Ctrl Pts',(-0.682543476113644,1.20366219176739,6.88122480138927));
#8389=CARTESIAN_POINT('Ctrl Pts',(-0.732386709520514,1.18278812258959,6.88122480138928));
#8390=CARTESIAN_POINT('Ctrl Pts',(-0.78082328725544,1.15871479259185,6.88122480138927));
#8391=CARTESIAN_POINT('Ctrl Pts',(-0.827721022731547,1.13172823854745,6.88122480138928));
#8392=CARTESIAN_POINT('Ctrl Pts',(-0.84745147406581,1.12037466495062,6.88122480138928));
#8393=CARTESIAN_POINT('Ctrl Pts',(-0.86690944613167,1.10850482371099,6.88122480138928));
#8394=CARTESIAN_POINT('Ctrl Pts',(-0.886084452197379,1.09613742275174,6.88122480138928));
#8395=CARTESIAN_POINT('Ctrl Pts',(-0.895254546003681,1.09022294081897,6.88122480138927));
#8396=CARTESIAN_POINT('Ctrl Pts',(-0.904359213369853,1.08419499716347,6.88122480138927));
#8397=CARTESIAN_POINT('Ctrl Pts',(-0.9133886633195,1.07806173785588,6.88122480138927));
#8398=CARTESIAN_POINT('Ctrl Pts',(-0.960084073216897,1.04634385260573,6.88122480138927));
#8399=CARTESIAN_POINT('Ctrl Pts',(-1.00483130342816,1.01177396154596,6.88122480138927));
#8400=CARTESIAN_POINT('Ctrl Pts',(-1.0474874886513,0.974668896684433,6.88122480138927));
#8401=CARTESIAN_POINT('Ctrl Pts',(-1.07964127198061,0.946699489440531,6.88122480138927));
#8402=CARTESIAN_POINT('Ctrl Pts',(-1.11060686174787,0.917288339612735,6.88122480138928));
#8403=CARTESIAN_POINT('Ctrl Pts',(-1.14031679043589,0.886552719621228,6.88122480138927));
#8404=CARTESIAN_POINT('Ctrl Pts',(-1.15037276608795,0.876149576297283,6.88122480138927));
#8405=CARTESIAN_POINT('Ctrl Pts',(-1.16028482946549,0.865594576601913,6.88122480138927));
#8406=CARTESIAN_POINT('Ctrl Pts',(-1.17005016216063,0.854891914773771,6.88122480138927));
#8407=CARTESIAN_POINT('Ctrl Pts',(-1.17927582847417,0.844780719407922,6.88122480138927));
#8408=CARTESIAN_POINT('Ctrl Pts',(-1.18837165555294,0.834536200457194,6.88122480138927));
#8409=CARTESIAN_POINT('Ctrl Pts',(-1.1973208397126,0.824179036166977,6.88122480138927));
#8410=CARTESIAN_POINT('Ctrl Pts',(-1.23576374944636,0.779687882023377,6.88122480138927));
#8411=CARTESIAN_POINT('Ctrl Pts',(-1.27156408809512,0.733055964514648,6.88122480138927));
#8412=CARTESIAN_POINT('Ctrl Pts',(-1.30457263970431,0.684606290778475,6.88122480138927));
#8413=CARTESIAN_POINT('Ctrl Pts',(-1.33817782711293,0.635280880046517,6.88122480138927));
#8414=CARTESIAN_POINT('Ctrl Pts',(-1.36889028667294,0.584070719971771,6.88122480138927));
#8415=CARTESIAN_POINT('Ctrl Pts',(-1.39652600638908,0.531270056701515,6.88122480138927));
#8416=CARTESIAN_POINT('Ctrl Pts',(-1.41410396658768,0.497685696787698,6.88122480138927));
#8417=CARTESIAN_POINT('Ctrl Pts',(-1.43043659202958,0.463456956653398,6.88122480138927));
#8418=CARTESIAN_POINT('Ctrl Pts',(-1.44546851334572,0.428652056108916,6.88122480138927));
#8419=CARTESIAN_POINT('Ctrl Pts',(-1.45233683119575,0.412749157560524,6.88122480138927));
#8420=CARTESIAN_POINT('Ctrl Pts',(-1.45893350142566,0.396725904291308,6.88122480138927));
#8421=CARTESIAN_POINT('Ctrl Pts',(-1.46525271318191,0.380588495018258,6.88122480138927));
#8422=CARTESIAN_POINT('Ctrl Pts',(-1.46896921857413,0.371097632725099,6.88122480138927));
#8423=CARTESIAN_POINT('Ctrl Pts',(-1.47258974601173,0.361567281164457,6.88122480138927));
#8424=CARTESIAN_POINT('Ctrl Pts',(-1.47611305419256,0.3519986756308,6.88122480138927));
#8425=CARTESIAN_POINT('Ctrl Pts',(-1.47979874984576,0.341989057961137,6.88122480138927));
#8426=CARTESIAN_POINT('Ctrl Pts',(-1.48337460810265,0.33194690923843,6.88122480138927));
#8427=CARTESIAN_POINT('Ctrl Pts',(-1.48683919026953,0.321875619808138,6.88122480138927));
#8428=CARTESIAN_POINT('Ctrl Pts',(-1.50680459825216,0.26383762483459,6.88122480138927));
#8429=CARTESIAN_POINT('Ctrl Pts',(-1.5230840690397,0.204817247296188,6.88122480138927));
#8430=CARTESIAN_POINT('Ctrl Pts',(-1.53549722234912,0.145128489083916,6.88122480138927));
#8431=CARTESIAN_POINT('Ctrl Pts',(-1.538454112368,0.13091025710066,6.88122480138927));
#8432=CARTESIAN_POINT('Ctrl Pts',(-1.54119145123912,0.116653938738659,6.88122480138927));
#8433=CARTESIAN_POINT('Ctrl Pts',(-1.54370646449436,0.10236349960097,6.88122480138927));
#8434=CARTESIAN_POINT('Ctrl Pts',(-1.55390853471807,0.0443947937474662,
6.88122480138927));
#8435=CARTESIAN_POINT('Ctrl Pts',(-1.56045619814385,-0.0141339339575868,
6.88122480138927));
#8436=CARTESIAN_POINT('Ctrl Pts',(-1.56350967632926,-0.0729601076848401,
6.88122480138927));
#8437=CARTESIAN_POINT('Ctrl Pts',(-1.56505061044946,-0.102646666013803,
6.88122480138927));
#8438=CARTESIAN_POINT('Ctrl Pts',(-1.56570089209292,-0.132409272280549,
6.88122480138927));
#8439=CARTESIAN_POINT('Ctrl Pts',(-1.5654763879049,-0.162215441966596,6.88122480138927));
#8440=CARTESIAN_POINT('Ctrl Pts',(-1.56533644256305,-0.180795204965318,
6.88122480138927));
#8441=CARTESIAN_POINT('Ctrl Pts',(-1.56485656325647,-0.199390994007395,
6.88122480138927));
#8442=CARTESIAN_POINT('Ctrl Pts',(-1.56403984705495,-0.217997968754189,
6.88122480138927));
#8443=CARTESIAN_POINT('Ctrl Pts',(-1.56345932716366,-0.231223761186564,
6.88122480138927));
#8444=CARTESIAN_POINT('Ctrl Pts',(-1.56270841160904,-0.244455267230033,
6.88122480138927));
#8445=CARTESIAN_POINT('Ctrl Pts',(-1.56179009164389,-0.257668068879168,
6.88122480138927));
#8446=CARTESIAN_POINT('Ctrl Pts',(-1.55754402835719,-0.318760492136378,
6.88122480138927));
#8447=CARTESIAN_POINT('Ctrl Pts',(-1.5497211828875,-0.379535249490823,6.88122480138927));
#8448=CARTESIAN_POINT('Ctrl Pts',(-1.53851766179682,-0.439705870790377,
6.88122480138927));
#8449=CARTESIAN_POINT('Ctrl Pts',(-1.52699040597737,-0.50161517045804,6.88122480138927));
#8450=CARTESIAN_POINT('Ctrl Pts',(-1.51188432995146,-0.562885842520045,
6.88122480138927));
#8451=CARTESIAN_POINT('Ctrl Pts',(-1.49335852869952,-0.623218541410667,
6.88122480138927));
#8452=CARTESIAN_POINT('Ctrl Pts',(-1.47483272744757,-0.68355124030129,6.88122480138927));
#8453=CARTESIAN_POINT('Ctrl Pts',(-1.45288698918659,-0.742947024621097,
6.88122480138927));
#8454=CARTESIAN_POINT('Ctrl Pts',(-1.42762827080073,-0.80110390561782,6.88122480138928));
#8455=CARTESIAN_POINT('Ctrl Pts',(-1.42298648268494,-0.811791380529987,
6.88122480138927));
#8456=CARTESIAN_POINT('Ctrl Pts',(-1.41823267413198,-0.822436983453104,
6.88122480138927));
#8457=CARTESIAN_POINT('Ctrl Pts',(-1.41336732622985,-0.833038785828612,
6.88122480138927));
#8458=CARTESIAN_POINT('Ctrl Pts',(-1.40898307425986,-0.84259225947229,6.88122480138927));
#8459=CARTESIAN_POINT('Ctrl Pts',(-1.40451005729422,-0.852106110738308,
6.88122480138927));
#8460=CARTESIAN_POINT('Ctrl Pts',(-1.39995239732874,-0.861571908632687,
6.88122480138927));
#8461=CARTESIAN_POINT('Ctrl Pts',(-1.37164075215683,-0.920372326672761,
6.88122480138927));
#8462=CARTESIAN_POINT('Ctrl Pts',(-1.34002926990105,-0.97740157812146,6.88122480138927));
#8463=CARTESIAN_POINT('Ctrl Pts',(-1.30529384686795,-1.03235040180416,6.88122480138927));
#8464=CARTESIAN_POINT('Ctrl Pts',(-1.27069709177016,-1.08707986325481,6.88122480138927));
#8465=CARTESIAN_POINT('Ctrl Pts',(-1.23300099244043,-1.13974654572362,6.88122480138928));
#8466=CARTESIAN_POINT('Ctrl Pts',(-1.19232907000199,-1.19003713909265,6.88122480138928));
#8467=CARTESIAN_POINT('Ctrl Pts',(-1.15202924701569,-1.23986763367317,6.88122480138928));
#8468=CARTESIAN_POINT('Ctrl Pts',(-1.10880748201239,-1.28736635050648,6.88122480138928));
#8469=CARTESIAN_POINT('Ctrl Pts',(-1.06273912028356,-1.33220527792149,6.88122480138928));
#8470=CARTESIAN_POINT('Ctrl Pts',(-1.0527315145224,-1.34194580898193,6.88122480138928));
#8471=CARTESIAN_POINT('Ctrl Pts',(-1.04258941726239,-1.35156070196631,6.88122480138927));
#8472=CARTESIAN_POINT('Ctrl Pts',(-1.03231334037779,-1.36104637311814,6.88122480138928));
#8473=CARTESIAN_POINT('Ctrl Pts',(-0.547737204315714,1.25137522550529,6.88122480138927));
#8474=CARTESIAN_POINT('Ctrl Pts',(-0.552435712024308,1.24931865012781,6.88141659114578));
#8475=CARTESIAN_POINT('Ctrl Pts',(-0.557122636949875,1.24723561241451,6.8816083809023));
#8476=CARTESIAN_POINT('Ctrl Pts',(-0.56179768176358,1.24512624450899,6.88180017065881));
#8477=CARTESIAN_POINT('Ctrl Pts',(0.748315817581761,1.5383870784886,2.15322551455621E-15));
#8478=CARTESIAN_POINT('Ctrl Pts',(0.79330974013975,1.51121254923536,2.00324072560254E-15));
#8479=CARTESIAN_POINT('Ctrl Pts',(0.83683948866918,1.48192024638845,2.72835309894076E-15));
#8480=CARTESIAN_POINT('Ctrl Pts',(0.878734943125877,1.45051315882962,1.8249290967276E-15));
#8481=CARTESIAN_POINT('Ctrl Pts',(0.930187061785903,1.41194188142498,7.84580135121318E-16));
#8482=CARTESIAN_POINT('Ctrl Pts',(0.979175755310881,1.37018143662514,2.88535685585316E-15));
#8483=CARTESIAN_POINT('Ctrl Pts',(1.02556564781079,1.32556170063658,2.99760216648792E-15));
#8484=CARTESIAN_POINT('Ctrl Pts',(1.07240876425823,1.28050603492728,3.11094410097838E-15));
#8485=CARTESIAN_POINT('Ctrl Pts',(1.11660252973995,1.23253384670277,9.75804439780424E-16));
#8486=CARTESIAN_POINT('Ctrl Pts',(1.15796154596301,1.18195995627099,1.7277845820729E-15));
#8487=CARTESIAN_POINT('Ctrl Pts',(1.17178013931695,1.16506255178646,1.97903107547438E-15));
#8488=CARTESIAN_POINT('Ctrl Pts',(1.18528187595262,1.14787458382087,2.54865482595334E-15));
#8489=CARTESIAN_POINT('Ctrl Pts',(1.19845856877168,1.13040751148756,1.48492329543615E-15));
#8490=CARTESIAN_POINT('Ctrl Pts',(1.20535439611853,1.12126637746256,9.04097576277068E-16));
#8491=CARTESIAN_POINT('Ctrl Pts',(1.21216118957793,1.11204880118057,1.55361878839882E-15));
#8492=CARTESIAN_POINT('Ctrl Pts',(1.21887770206587,1.10275642073377,2.51187959321442E-15));
#8493=CARTESIAN_POINT('Ctrl Pts',(1.2257756336561,1.09321304465169,3.19792110923887E-15));
#8494=CARTESIAN_POINT('Ctrl Pts',(1.23257353957357,1.08359733938013,3.17391878255083E-15));
#8495=CARTESIAN_POINT('Ctrl Pts',(1.23926703280866,1.07391651229646,3.08780778723872E-15));
#8496=CARTESIAN_POINT('Ctrl Pts',(1.27551793785583,1.02148667767015,2.571274784078E-15));
#8497=CARTESIAN_POINT('Ctrl Pts',(1.30874446989807,0.967101148680756,6.0414663234747E-16));
#8498=CARTESIAN_POINT('Ctrl Pts',(1.338811224237,0.911076311564746,1.38777878078145E-15));
#8499=CARTESIAN_POINT('Ctrl Pts',(1.3702518095946,0.852491548685597,2.20721719352362E-15));
#8500=CARTESIAN_POINT('Ctrl Pts',(1.39823810519405,0.79211305995548,-1.27615658727163E-16));
#8501=CARTESIAN_POINT('Ctrl Pts',(1.42255628167792,0.730287083244153,2.35922392732846E-16));
#8502=CARTESIAN_POINT('Ctrl Pts',(1.44502502073072,0.673163074035149,5.71812775773418E-16));
#8503=CARTESIAN_POINT('Ctrl Pts',(1.46436199499226,0.614802389501134,-4.25826032830452E-15));
#8504=CARTESIAN_POINT('Ctrl Pts',(1.48034796790375,0.555481066013023,2.77555756156289E-17));
#8505=CARTESIAN_POINT('Ctrl Pts',(1.48166379860548,0.55059823409877,3.80544320203479E-16));
#8506=CARTESIAN_POINT('Ctrl Pts',(1.48295689684359,0.545708899972741,7.86156538718846E-16));
#8507=CARTESIAN_POINT('Ctrl Pts',(1.48422712470284,0.540813221486026,1.41553435639707E-15));
#8508=CARTESIAN_POINT('Ctrl Pts',(1.4867316679211,0.531160277517357,2.65882271871602E-15));
#8509=CARTESIAN_POINT('Ctrl Pts',(1.48914639934276,0.521485933259116,2.32141274649425E-15));
#8510=CARTESIAN_POINT('Ctrl Pts',(1.49146863316748,0.511799559522065,2.23432383705813E-15));
#8511=CARTESIAN_POINT('Ctrl Pts',(1.50564287428223,0.452676746214071,2.4148937701561E-15));
#8512=CARTESIAN_POINT('Ctrl Pts',(1.51639877554924,0.393016146915013,2.33379373485162E-15));
#8513=CARTESIAN_POINT('Ctrl Pts',(1.52358166896565,0.333090755615199,9.29811783123569E-16));
#8514=CARTESIAN_POINT('Ctrl Pts',(1.53054106613352,0.27502994720298,-1.32152166187657E-15));
#8515=CARTESIAN_POINT('Ctrl Pts',(1.53414632425553,0.216719733480015,-1.71265129966507E-15));
#8516=CARTESIAN_POINT('Ctrl Pts',(1.53420883231942,0.158413996521009,-4.44089209850063E-16));
#8517=CARTESIAN_POINT('Ctrl Pts',(1.53424500829747,0.124670077262913,4.98577800183531E-16));
#8518=CARTESIAN_POINT('Ctrl Pts',(1.53309367734275,0.0909278273352152,-6.71329225516391E-16));
#8519=CARTESIAN_POINT('Ctrl Pts',(1.53071060824393,0.0572389507155212,-9.85322934354826E-16));
#8520=CARTESIAN_POINT('Ctrl Pts',(1.52842944993871,0.0249907625566291,-1.07107518135246E-15));
#8521=CARTESIAN_POINT('Ctrl Pts',(1.52501947762763,-0.00720854617748223,
-2.07868045293857E-15));
#8522=CARTESIAN_POINT('Ctrl Pts',(1.52050115185295,-0.0393112549066445,
-2.06779038336435E-15));
#8523=CARTESIAN_POINT('Ctrl Pts',(1.51864265927286,-0.0525158463745993,
-1.87592535676816E-15));
#8524=CARTESIAN_POINT('Ctrl Pts',(1.51659588303773,-0.0657074995902743,
-1.62350288100921E-15));
#8525=CARTESIAN_POINT('Ctrl Pts',(1.5143668392248,-0.0788573464476957,-1.70696790036118E-15));
#8526=CARTESIAN_POINT('Ctrl Pts',(1.5045273247336,-0.136903809222598,-2.16891961470101E-15));
#8527=CARTESIAN_POINT('Ctrl Pts',(1.49112862123246,-0.194234466941921,-2.81475207116788E-15));
#8528=CARTESIAN_POINT('Ctrl Pts',(1.47436851148242,-0.250588170236329,-1.1518563880486E-15));
#8529=CARTESIAN_POINT('Ctrl Pts',(1.4568136293047,-0.309614193118367,5.89894604418642E-16));
#8530=CARTESIAN_POINT('Ctrl Pts',(1.43557050341456,-0.367569697988627,3.94366376571076E-16));
#8531=CARTESIAN_POINT('Ctrl Pts',(1.41081400323684,-0.424124826119812,3.05311331771918E-16));
#8532=CARTESIAN_POINT('Ctrl Pts',(1.38734333111861,-0.47774253700151,2.20881717652363E-16));
#8533=CARTESIAN_POINT('Ctrl Pts',(1.36071371363536,-0.530102124474644,-3.10126693863359E-16));
#8534=CARTESIAN_POINT('Ctrl Pts',(1.33104076585779,-0.580883676744975,-2.3037127760972E-15));
#8535=CARTESIAN_POINT('Ctrl Pts',(1.32941514948567,-0.583665716581097,-2.41293030981866E-15));
#8536=CARTESIAN_POINT('Ctrl Pts',(1.32778039253364,-0.586443008841638,-2.36550771100398E-15));
#8537=CARTESIAN_POINT('Ctrl Pts',(1.32613651184916,-0.589215496846285,-2.44249065417534E-15));
#8538=CARTESIAN_POINT('Ctrl Pts',(1.32062943215923,-0.598503465568777,-2.53258028311659E-15));
#8539=CARTESIAN_POINT('Ctrl Pts',(1.31502183376448,-0.607734246301079,-2.0661488452891E-15));
#8540=CARTESIAN_POINT('Ctrl Pts',(1.30931903080635,-0.616898915910521,-1.99840144432528E-15));
#8541=CARTESIAN_POINT('Ctrl Pts',(1.27896983478356,-0.665671485557963,-1.81941077559367E-15));
#8542=CARTESIAN_POINT('Ctrl Pts',(1.24589105028342,-0.712635601535066,-7.13006852229392E-16));
#8543=CARTESIAN_POINT('Ctrl Pts',(1.210222326866,-0.757511300638567,-5.55111512312578E-16));
#8544=CARTESIAN_POINT('Ctrl Pts',(1.1802861081694,-0.79517479441724,-4.22592347788311E-16));
#8545=CARTESIAN_POINT('Ctrl Pts',(1.14852468994335,-0.831366862692395,-1.65660898229942E-15));
#8546=CARTESIAN_POINT('Ctrl Pts',(1.11500605367636,-0.865897589688669,-1.27675647831893E-15));
#8547=CARTESIAN_POINT('Ctrl Pts',(1.106788817097,-0.874362944625117,-1.34173175461127E-15));
#8548=CARTESIAN_POINT('Ctrl Pts',(1.09846592082978,-0.882728332671732,-1.4518904375016E-15));
#8549=CARTESIAN_POINT('Ctrl Pts',(1.09003827756787,-0.890990714153347,-6.93889390390723E-16));
#8550=CARTESIAN_POINT('Ctrl Pts',(1.08120696979645,-0.8996488444896,1.26881278685788E-16));
#8551=CARTESIAN_POINT('Ctrl Pts',(1.07226667800469,-0.908187904030433,-9.62861165954058E-16));
#8552=CARTESIAN_POINT('Ctrl Pts',(1.0632213738949,-0.916602560539565,-5.82867087928207E-16));
#8553=CARTESIAN_POINT('Ctrl Pts',(1.02245569976267,-0.95452601131826,1.67515078953523E-15));
#8554=CARTESIAN_POINT('Ctrl Pts',(0.979542146270061,-0.989942845515599,
-2.99196435015932E-16));
#8555=CARTESIAN_POINT('Ctrl Pts',(0.934596947466491,-1.02256508694638,5.82867087928207E-16));
#8556=CARTESIAN_POINT('Ctrl Pts',(0.889651748662921,-1.05518732837715,1.58939179805206E-15));
#8557=CARTESIAN_POINT('Ctrl Pts',(0.842674238566416,-1.08501566506116,-2.12027705394649E-16));
#8558=CARTESIAN_POINT('Ctrl Pts',(0.793764246391153,-1.11170783983522,-5.82867087928207E-16));
#8559=CARTESIAN_POINT('Origin',(0.,0.,8.66831010612084));
#8560=CARTESIAN_POINT('',(-2.72578406873475,-3.33812273494286E-16,8.66831010612084));
#8561=CARTESIAN_POINT('Origin',(0.,0.,8.66831010612084));
#8562=CARTESIAN_POINT('Origin',(1.80562831587628,0.,0.));
#8563=CARTESIAN_POINT('Origin',(3.51922397520286,0.,6.88122480138927));
#8564=CARTESIAN_POINT('',(-3.51922397520286,-4.30980637671481E-16,6.88122480138927));
#8565=CARTESIAN_POINT('Origin',(0.,0.,6.88122480138927));
#8566=CARTESIAN_POINT('Origin',(0.,0.,8.31887564143431));
#8567=CARTESIAN_POINT('',(-3.51922397520286,-4.30980637671481E-16,9.75652648147935));
#8568=CARTESIAN_POINT('Origin',(0.,0.,9.75652648147935));
#8569=CARTESIAN_POINT('',(-3.51922397520286,-4.30980637671481E-16,8.31887564143431));
#8570=CARTESIAN_POINT('Origin',(0.,0.,9.84316232611724));
#8571=CARTESIAN_POINT('',(-3.18037436229666,-3.8948352828769E-16,9.92979817075513));
#8572=CARTESIAN_POINT('',(-3.34979916874976,4.10232082979586E-16,9.84316232611724));
#8573=CARTESIAN_POINT('Origin',(0.,0.,9.92979817075513));
#8574=CARTESIAN_POINT('Origin',(0.,0.,10.7561296768773));
#8575=CARTESIAN_POINT('',(-3.18037436229666,-3.8948352828769E-16,11.5824611829994));
#8576=CARTESIAN_POINT('Origin',(0.,0.,11.5824611829994));
#8577=CARTESIAN_POINT('',(-3.18037436229666,-3.89483528287691E-16,10.7561296768773));
#8578=CARTESIAN_POINT('Origin',(3.71701820384649,0.,11.5824611829994));
#8579=CARTESIAN_POINT('',(-3.71701820384649,-4.55203444571304E-16,11.5824611829994));
#8580=CARTESIAN_POINT('Origin',(0.,0.,11.5824611829994));
#8581=CARTESIAN_POINT('Origin',(0.,0.,12.6961282806954));
#8582=CARTESIAN_POINT('',(-3.71701820384649,-4.55203444571304E-16,13.8097953783913));
#8583=CARTESIAN_POINT('Origin',(0.,0.,13.8097953783913));
#8584=CARTESIAN_POINT('',(-3.71701820384649,-4.55203444571305E-16,12.6961282806954));
#8585=CARTESIAN_POINT('Origin',(0.,0.,13.8097953783913));
#8586=CARTESIAN_POINT('',(-3.01701820384649,-3.6947816863099E-16,14.5097953783913));
#8587=CARTESIAN_POINT('Origin',(0.,0.,14.5097953783913));
#8588=CARTESIAN_POINT('Origin',(-3.01701820384648,-3.69478168630989E-16,
13.8097953783913));
#8589=CARTESIAN_POINT('Origin',(1.4890246697361,0.,14.5097953783913));
#8590=CARTESIAN_POINT('',(-1.4890246697361,-1.82352929564375E-16,14.5097953783913));
#8591=CARTESIAN_POINT('Origin',(0.,0.,14.5097953783913));
#8592=CARTESIAN_POINT('Origin',(0.,0.,14.1858997942285));
#8593=CARTESIAN_POINT('',(-1.4890246697361,-1.82352929564375E-16,13.8620042100656));
#8594=CARTESIAN_POINT('Origin',(0.,0.,13.8620042100656));
#8595=CARTESIAN_POINT('',(-1.4890246697361,-1.82352929564376E-16,14.1858997942285));
#8596=CARTESIAN_POINT('Origin',(2.72578406873475,0.,13.8620042100656));
#8597=CARTESIAN_POINT('',(-2.72578406873475,-3.33812273494286E-16,13.8620042100656));
#8598=CARTESIAN_POINT('Origin',(0.,0.,13.8620042100656));
#8599=CARTESIAN_POINT('Origin',(0.,0.,11.2651571580932));
#8600=CARTESIAN_POINT('',(-2.72578406873475,-3.33812273494286E-16,11.2651571580932));
#8601=CARTESIAN_POINT('',(0.,0.,0.));
#8602=CARTESIAN_POINT('Origin',(6.73223109314486,0.,86.2971179986903));
#8603=CARTESIAN_POINT('',(-6.73223109314486,-8.24460525934014E-16,86.2971179986903));
#8604=CARTESIAN_POINT('Origin',(0.,0.,86.2971179986903));
#8605=CARTESIAN_POINT('',(-1.77103530981268,-2.16889272333904E-16,86.2971179986903));
#8606=CARTESIAN_POINT('Origin',(0.,0.,86.2971179986903));
#8607=CARTESIAN_POINT('Origin',(0.,0.,86.0650263196877));
#8608=CARTESIAN_POINT('',(-7.15220058470855,-8.75891955292316E-16,85.8329346406852));
#8609=CARTESIAN_POINT('',(-6.94221583892671,8.50176240613165E-16,86.0650263196877));
#8610=CARTESIAN_POINT('Origin',(0.,0.,85.8329346406852));
#8611=CARTESIAN_POINT('Origin',(9.55065635544564,0.,85.8329346406852));
#8612=CARTESIAN_POINT('',(-9.55065635544564,-1.16961807354528E-15,85.8329346406852));
#8613=CARTESIAN_POINT('Origin',(0.,0.,85.8329346406852));
#8614=CARTESIAN_POINT('Origin',(0.,0.,86.0940133608864));
#8615=CARTESIAN_POINT('',(-10.0021025234003,-1.22490428400259E-15,86.3550920810876));
#8616=CARTESIAN_POINT('Origin',(0.,0.,86.3550920810876));
#8617=CARTESIAN_POINT('',(-9.77637943942299,-1.19726117877394E-15,86.0940133608864));
#8618=CARTESIAN_POINT('Origin',(11.3384150169577,0.,86.3550920810876));
#8619=CARTESIAN_POINT('',(-11.3384150169577,-1.38855536579215E-15,86.3550920810876));
#8620=CARTESIAN_POINT('Origin',(0.,0.,86.3550920810876));
#8621=CARTESIAN_POINT('Origin',(0.,0.,86.8168854949443));
#8622=CARTESIAN_POINT('',(-11.3384150169577,-1.38855536579215E-15,87.278678908801));
#8623=CARTESIAN_POINT('Origin',(0.,0.,87.278678908801));
#8624=CARTESIAN_POINT('',(-11.3384150169577,-1.38855536579215E-15,86.8168854949443));
#8625=CARTESIAN_POINT('Origin',(0.,0.,87.4271189254628));
#8626=CARTESIAN_POINT('',(-10.9691252194088,-1.34333040893955E-15,87.5755589421246));
#8627=CARTESIAN_POINT('',(-11.1537701181833,1.36594288736586E-15,87.4271189254628));
#8628=CARTESIAN_POINT('Origin',(0.,0.,87.5755589421246));
#8629=CARTESIAN_POINT('Origin',(8.63028983493237,0.,87.5755589421246));
#8630=CARTESIAN_POINT('',(-8.63028983493237,-1.05690568220639E-15,87.5755589421246));
#8631=CARTESIAN_POINT('Origin',(0.,0.,87.5755589421246));
#8632=CARTESIAN_POINT('Origin',(0.,0.,88.1584575441381));
#8633=CARTESIAN_POINT('',(-7.86274633414444,-9.62908713061757E-16,88.7413561461516));
#8634=CARTESIAN_POINT('',(-8.2465180845384,1.00990719763407E-15,88.1584575441381));
#8635=CARTESIAN_POINT('Origin',(0.,0.,88.7413561461516));
#8636=CARTESIAN_POINT('Origin',(6.03157539652109,0.,88.7413561461516));
#8637=CARTESIAN_POINT('',(-6.03157539652109,-7.38654950316548E-16,88.7413561461516));
#8638=CARTESIAN_POINT('Origin',(0.,0.,88.7413561461516));
#8639=CARTESIAN_POINT('Origin',(0.,0.,92.3318522386825));
#8640=CARTESIAN_POINT('',(-6.03157539652109,-7.38654950316548E-16,95.9223483312135));
#8641=CARTESIAN_POINT('Origin',(0.,0.,95.9223483312135));
#8642=CARTESIAN_POINT('',(-6.03157539652109,-7.38654950316548E-16,92.3318522386825));
#8643=CARTESIAN_POINT('Origin',(4.0030788546633,0.,95.9223483312135));
#8644=CARTESIAN_POINT('',(-4.0030788546633,-4.90235770609787E-16,95.9223483312135));
#8645=CARTESIAN_POINT('Origin',(0.,0.,95.9223483312135));
#8646=CARTESIAN_POINT('Origin',(0.,0.,95.536476432406));
#8647=CARTESIAN_POINT('',(-3.80367971583355,-4.65816418897727E-16,95.1506045335986));
#8648=CARTESIAN_POINT('Origin',(0.,0.,95.1506045335986));
#8649=CARTESIAN_POINT('',(-3.90337928524842,-4.78026094753756E-16,95.536476432406));
#8650=CARTESIAN_POINT('Origin',(2.91473371720024,0.,95.1506045335986));
#8651=CARTESIAN_POINT('',(-2.91473371720024,-3.56951931713614E-16,95.1506045335986));
#8652=CARTESIAN_POINT('Origin',(0.,0.,95.1506045335986));
#8653=CARTESIAN_POINT('Origin',(0.,0.,93.4125396072643));
#8654=CARTESIAN_POINT('',(-2.91473371720024,-3.56951931713614E-16,91.6744746809301));
#8655=CARTESIAN_POINT('Origin',(0.,0.,91.6744746809301));
#8656=CARTESIAN_POINT('',(-2.91473371720024,-3.56951931713614E-16,93.4125396072643));
#8657=CARTESIAN_POINT('Origin',(2.52802020062926,0.,91.6744746809301));
#8658=CARTESIAN_POINT('',(-2.52802020062926,-3.09593184688047E-16,91.6744746809301));
#8659=CARTESIAN_POINT('Origin',(0.,0.,91.6744746809301));
#8660=CARTESIAN_POINT('Origin',(0.,0.,90.2007950732064));
#8661=CARTESIAN_POINT('',(-2.52802020062926,-3.09593184688047E-16,88.7271154654827));
#8662=CARTESIAN_POINT('Origin',(0.,0.,88.7271154654827));
#8663=CARTESIAN_POINT('',(-2.52802020062926,-3.09593184688047E-16,90.2007950732064));
#8664=CARTESIAN_POINT('Origin',(0.,0.,88.5025936415912));
#8665=CARTESIAN_POINT('',(-1.77103530981268,-2.16889272333904E-16,88.2780718176998));
#8666=CARTESIAN_POINT('Origin',(0.,0.,88.2780718176998));
#8667=CARTESIAN_POINT('',(-2.14952775522097,-2.63241228510976E-16,88.5025936415912));
#8668=CARTESIAN_POINT('Origin',(0.,0.,87.287594908195));
#8669=CARTESIAN_POINT('',(-1.77103530981268,-2.16889272333904E-16,87.287594908195));
#8670=CARTESIAN_POINT('',(0.,0.,0.));
#8671=CARTESIAN_POINT('Origin',(0.,0.,89.2710285354474));
#8672=CARTESIAN_POINT('',(-1.66796412351461,1.09611534438488,91.3549851603904));
#8673=CARTESIAN_POINT('',(-1.66701720873947,1.09548217158769,91.1951011757363));
#8674=CARTESIAN_POINT('',(-1.66701720851066,1.09548217193587,89.2710285354474));
#8675=CARTESIAN_POINT('',(-1.16224713396736,-1.62528722506882,90.7501273547608));
#8676=CARTESIAN_POINT('Ctrl Pts',(-1.16224713396736,-1.62528722506882,90.7501273547608));
#8677=CARTESIAN_POINT('Ctrl Pts',(-0.658524710503023,-1.98155496728916,
90.7896669606139));
#8678=CARTESIAN_POINT('Ctrl Pts',(0.758122744768261,-2.20830555489497,90.8716287779614));
#8679=CARTESIAN_POINT('Ctrl Pts',(2.27985988398632,-0.606850097788344,90.9960128068036));
#8680=CARTESIAN_POINT('Ctrl Pts',(1.74311916661052,1.59020182115508,91.1232794412872));
#8681=CARTESIAN_POINT('Ctrl Pts',(-0.267372268586595,2.28195004315838,91.2429368924828));
#8682=CARTESIAN_POINT('Ctrl Pts',(-1.36442438513313,1.54816875793513,91.3201721321838));
#8683=CARTESIAN_POINT('Ctrl Pts',(-1.66796412351456,1.09611534438494,91.3549851603904));
#8684=CARTESIAN_POINT('',(1.16034898466941,-1.62253437445148,90.7500736540522));
#8685=CARTESIAN_POINT('Origin',(0.,0.,90.7500736540522));
#8686=CARTESIAN_POINT('Ctrl Pts',(1.16034898466941,-1.62253437445149,90.7500736540522));
#8687=CARTESIAN_POINT('Ctrl Pts',(1.17314904347898,-1.61338046346059,90.7510781037149));
#8688=CARTESIAN_POINT('Ctrl Pts',(1.18584074592424,-1.6040751090438,90.7520741371569));
#8689=CARTESIAN_POINT('Ctrl Pts',(1.21629818685645,-1.58118511405926,90.754467732357));
#8690=CARTESIAN_POINT('Ctrl Pts',(1.23394844976023,-1.56744982135387,90.7558576320957));
#8691=CARTESIAN_POINT('Ctrl Pts',(1.31553677040832,-1.50172597808865,90.7623129882304));
#8692=CARTESIAN_POINT('Ctrl Pts',(1.37644870744073,-1.44610123818527,90.767223643896));
#8693=CARTESIAN_POINT('Ctrl Pts',(1.4998823884772,-1.31849477652871,90.7777600138677));
#8694=CARTESIAN_POINT('Ctrl Pts',(1.56103893598951,-1.24548474182317,90.783368483509));
#8695=CARTESIAN_POINT('Ctrl Pts',(1.64770706696334,-1.12555848729566,90.7923069388478));
#8696=CARTESIAN_POINT('Ctrl Pts',(1.67694569491042,-1.08151422923847,90.7955369743538));
#8697=CARTESIAN_POINT('Ctrl Pts',(1.71942535119665,-1.0116523248723,90.8006218826066));
#8698=CARTESIAN_POINT('Ctrl Pts',(1.73391115998772,-0.986618432168437,90.8024365599979));
#8699=CARTESIAN_POINT('Ctrl Pts',(1.76046404777739,-0.938338619060236,90.8059284417133));
#8700=CARTESIAN_POINT('Ctrl Pts',(1.77262762735366,-0.915152568354784,90.807602042306));
#8701=CARTESIAN_POINT('Ctrl Pts',(1.80019886612251,-0.859983450464937,90.8115805946841));
#8702=CARTESIAN_POINT('Ctrl Pts',(1.81521562543524,-0.827816085726226,90.8138976352077));
#8703=CARTESIAN_POINT('Ctrl Pts',(1.87080253475281,-0.699948587126537,90.8231081504074));
#8704=CARTESIAN_POINT('Ctrl Pts',(1.90472058368382,-0.601551410959497,90.830206909549));
#8705=CARTESIAN_POINT('Ctrl Pts',(1.95976016705419,-0.389421489844373,90.8454705237484));
#8706=CARTESIAN_POINT('Ctrl Pts',(1.97898141212054,-0.275574199166582,90.8536406166416));
#8707=CARTESIAN_POINT('Ctrl Pts',(1.99134355319383,-0.122628503092087,90.8642704219524));
#8708=CARTESIAN_POINT('Ctrl Pts',(1.99332693643587,-0.0844686511425707,
90.8668926891416));
#8709=CARTESIAN_POINT('Ctrl Pts',(1.99486942905621,-0.0179928339290739,
90.8713866626133));
#8710=CARTESIAN_POINT('Ctrl Pts',(1.99492402917294,0.0103002136719869,90.8732759972948));
#8711=CARTESIAN_POINT('Ctrl Pts',(1.99408286963858,0.0537762631839919,90.8761345895388));
#8712=CARTESIAN_POINT('Ctrl Pts',(1.99361544708385,0.0689627639697828,90.8771247363347));
#8713=CARTESIAN_POINT('Ctrl Pts',(1.99241544078782,0.0973855824031539,90.8789604738342));
#8714=CARTESIAN_POINT('Ctrl Pts',(1.9917244097925,0.110621563021882,90.8798080400829));
#8715=CARTESIAN_POINT('Ctrl Pts',(1.98964201244626,0.144096074229982,90.8819342362994));
#8716=CARTESIAN_POINT('Ctrl Pts',(1.98807379735177,0.164321854025372,90.8832031574842));
#8717=CARTESIAN_POINT('Ctrl Pts',(1.97943171953755,0.257345723261733,90.8889816870942));
#8718=CARTESIAN_POINT('Ctrl Pts',(1.96866533397623,0.329751118414626,90.8933178064752));
#8719=CARTESIAN_POINT('Ctrl Pts',(1.92307623920396,0.551666289816138,90.9065569507854));
#8720=CARTESIAN_POINT('Ctrl Pts',(1.87498178573657,0.697854286959789,90.9152481262817));
#8721=CARTESIAN_POINT('Ctrl Pts',(1.79306404781305,0.875041254201998,90.9270025640284));
#8722=CARTESIAN_POINT('Ctrl Pts',(1.77432955902559,0.91243087898068,90.9295542663064));
#8723=CARTESIAN_POINT('Ctrl Pts',(1.74273613999407,0.970825807503868,90.9336728607101));
#8724=CARTESIAN_POINT('Ctrl Pts',(1.73063888479634,0.992230297683102,90.9352119720363));
#8725=CARTESIAN_POINT('Ctrl Pts',(1.70665945207541,1.03288556610933,90.9381957212619));
#8726=CARTESIAN_POINT('Ctrl Pts',(1.69483929904236,1.0521685967344,90.9396378370712));
#8727=CARTESIAN_POINT('Ctrl Pts',(1.66620630845414,1.09714479854448,90.9430677896392));
#8728=CARTESIAN_POINT('Ctrl Pts',(1.64912349622755,1.12265831047906,90.945065945843));
#8729=CARTESIAN_POINT('Ctrl Pts',(1.58692178572088,1.21107315235884,90.9521825386533));
#8730=CARTESIAN_POINT('Ctrl Pts',(1.53874260466519,1.27172618677324,90.9574205389424));
#8731=CARTESIAN_POINT('Ctrl Pts',(1.40000286675475,1.42692845832341,90.9717871906183));
#8732=CARTESIAN_POINT('Ctrl Pts',(1.30346770152365,1.51561912863029,90.981090801111));
#8733=CARTESIAN_POINT('Ctrl Pts',(1.16757685224896,1.61781736669191,90.9928981266502));
#8734=CARTESIAN_POINT('Ctrl Pts',(1.13551000684884,1.64048350387597,90.9955994120794));
#8735=CARTESIAN_POINT('Ctrl Pts',(1.07911858449896,1.67789685365977,91.000179808331));
#8736=CARTESIAN_POINT('Ctrl Pts',(1.05510942687394,1.69309747947808,91.0020792901247));
#8737=CARTESIAN_POINT('Ctrl Pts',(1.01826336814747,1.71533702009854,91.0049089206537));
#8738=CARTESIAN_POINT('Ctrl Pts',(1.00566121657515,1.7227556231055,91.0058619639392));
#8739=CARTESIAN_POINT('Ctrl Pts',(0.981510112217735,1.7366174882257,91.007658760689));
#8740=CARTESIAN_POINT('Ctrl Pts',(0.969976617984684,1.74308570822472,91.0085042286633));
#8741=CARTESIAN_POINT('Ctrl Pts',(0.941019432878275,1.75894905954882,91.0105978384044));
#8742=CARTESIAN_POINT('Ctrl Pts',(0.923518224841293,1.76820064682644,91.0118372017672));
#8743=CARTESIAN_POINT('Ctrl Pts',(0.851419248788649,1.80495141625567,91.0168495666815));
#8744=CARTESIAN_POINT('Ctrl Pts',(0.795704518339729,1.83019672626533,91.0205071714274));
#8745=CARTESIAN_POINT('Ctrl Pts',(0.619851178851142,1.9003269259806,91.0316569500777));
#8746=CARTESIAN_POINT('Ctrl Pts',(0.496488873647193,1.93622270316455,91.0389470664234));
#8747=CARTESIAN_POINT('Ctrl Pts',(0.322734561577925,1.96906989514896,91.0493616947144));
#8748=CARTESIAN_POINT('Ctrl Pts',(0.27462470607308,1.97635388295567,91.052257680539));
#8749=CARTESIAN_POINT('Ctrl Pts',(0.186967611432868,1.98636295532512,91.0575979725878));
#8750=CARTESIAN_POINT('Ctrl Pts',(0.147513622281268,1.98968190605767,91.0600246697606));
#8751=CARTESIAN_POINT('Ctrl Pts',(0.0829610438155578,1.99318169362283,91.0640471674946));
#8752=CARTESIAN_POINT('Ctrl Pts',(0.057910770585411,1.99406671158738,91.0656208336947));
#8753=CARTESIAN_POINT('Ctrl Pts',(0.00878138519335234,1.99487592846905,
91.0687351396053));
#8754=CARTESIAN_POINT('Ctrl Pts',(-0.015292867076133,1.9948366167766,91.0702743640615));
#8755=CARTESIAN_POINT('Ctrl Pts',(-0.0747348504066648,1.99366350093632,
91.0741097205133));
#8756=CARTESIAN_POINT('Ctrl Pts',(-0.110083193392411,1.99202431754119,91.076421073309));
#8757=CARTESIAN_POINT('Ctrl Pts',(-0.286286550827132,1.97914925676344,91.0881016207235));
#8758=CARTESIAN_POINT('Ctrl Pts',(-0.425692903973189,1.95391031228548,91.0978923727981));
#8759=CARTESIAN_POINT('Ctrl Pts',(-0.645225208120578,1.88954278972236,91.1138013561186));
#8760=CARTESIAN_POINT('Ctrl Pts',(-0.727505616938371,1.85941533891063,91.1198722607316));
#8761=CARTESIAN_POINT('Ctrl Pts',(-0.830580501290487,1.81378008056937,91.1274266453653));
#8762=CARTESIAN_POINT('Ctrl Pts',(-0.85342091740846,1.80314586879498,91.1290969117543));
#8763=CARTESIAN_POINT('Ctrl Pts',(-0.889209964017591,1.78565047319742,91.1317013172632));
#8764=CARTESIAN_POINT('Ctrl Pts',(-0.902294280195474,1.77907476977465,91.1326507195481));
#8765=CARTESIAN_POINT('Ctrl Pts',(-0.926546287624919,1.76655019596719,91.1344036387738));
#8766=CARTESIAN_POINT('Ctrl Pts',(-0.937731827196888,1.76063813753127,91.1352093013974));
#8767=CARTESIAN_POINT('Ctrl Pts',(-0.968624676250945,1.7439319511873,91.1374286153975));
#8768=CARTESIAN_POINT('Ctrl Pts',(-0.988207730889158,1.73291026721569,91.1388288278613));
#8769=CARTESIAN_POINT('Ctrl Pts',(-1.1195732026294,1.65602415182174,91.148205074385));
#8770=CARTESIAN_POINT('Ctrl Pts',(-1.22489847674672,1.5797126952943,91.1556545804726));
#8771=CARTESIAN_POINT('Ctrl Pts',(-1.40112681167,1.42373319352022,91.1693229533324));
#8772=CARTESIAN_POINT('Ctrl Pts',(-1.47449274185012,1.34760555965701,91.1754898202527));
#8773=CARTESIAN_POINT('Ctrl Pts',(-1.56504129653026,1.23735627940756,91.1841572987751));
#8774=CARTESIAN_POINT('Ctrl Pts',(-1.58778915038505,1.20802738662344,91.186439273085));
#8775=CARTESIAN_POINT('Ctrl Pts',(-1.62419313020345,1.15828582795485,91.1902829347968));
#8776=CARTESIAN_POINT('Ctrl Pts',(-1.63831456820407,1.13822435096106,91.1918262475269));
#8777=CARTESIAN_POINT('Ctrl Pts',(-1.6570976652941,1.11046640179257,91.1939544134049));
#8778=CARTESIAN_POINT('Ctrl Pts',(-1.66208285755213,1.10299087283048,91.1945268467398));
#8779=CARTESIAN_POINT('Ctrl Pts',(-1.66701720873947,1.09548217158769,91.1951011757363));
#8780=CARTESIAN_POINT('Origin',(0.,0.,89.2710285354474));
#8781=CARTESIAN_POINT('',(-1.66701720851066,1.09548217193587,92.1551526428301));
#8782=CARTESIAN_POINT('',(-1.66701737487201,1.09548191878042,91.9972724317));
#8783=CARTESIAN_POINT('',(-1.66701720851066,1.09548217193587,89.2710285354474));
#8784=CARTESIAN_POINT('',(-1.99466808022928,0.0010228270418267,91.429118747959));
#8785=CARTESIAN_POINT('Ctrl Pts',(-1.9947497379454,0.00102248069035476,
91.429118772657));
#8786=CARTESIAN_POINT('Ctrl Pts',(-1.99478604894113,-0.06981636243393,91.4336193689785));
#8787=CARTESIAN_POINT('Ctrl Pts',(-1.99104450452175,-0.140650429119896,
91.4381199653));
#8788=CARTESIAN_POINT('Ctrl Pts',(-1.98355300646027,-0.211056942701271,
91.4426205616215));
#8789=CARTESIAN_POINT('Ctrl Pts',(-1.97605859417038,-0.281490844751671,
91.4471229086964));
#8790=CARTESIAN_POINT('Ctrl Pts',(-1.96481138056007,-0.351496395942167,
91.4516252557713));
#8791=CARTESIAN_POINT('Ctrl Pts',(-1.94989092191128,-0.420657764873042,
91.4561276028462));
#8792=CARTESIAN_POINT('Ctrl Pts',(-1.93494812103891,-0.489922697561851,
91.4606366918348));
#8793=CARTESIAN_POINT('Ctrl Pts',(-1.91632119468705,-0.55834046408667,91.4651457808234));
#8794=CARTESIAN_POINT('Ctrl Pts',(-1.89414034210309,-0.62550773529796,91.469654869812));
#8795=CARTESIAN_POINT('Ctrl Pts',(-1.87194157105775,-0.69272926655858,91.474167601399));
#8796=CARTESIAN_POINT('Ctrl Pts',(-1.84618332850722,-0.758697853304446,
91.478680332986));
#8797=CARTESIAN_POINT('Ctrl Pts',(-1.81704398589159,-0.823030203476888,
91.4831930645729));
#8798=CARTESIAN_POINT('Ctrl Pts',(-1.7878445441515,-0.887495237422273,91.4877151035496));
#8799=CARTESIAN_POINT('Ctrl Pts',(-1.75525029179399,-0.950316877422571,
91.4922371425263));
#8800=CARTESIAN_POINT('Ctrl Pts',(-1.71948537196905,-1.01113679494144,91.4967591815029));
#8801=CARTESIAN_POINT('Ctrl Pts',(-1.6975505786476,-1.04843793603541,91.499532569248));
#8802=CARTESIAN_POINT('Ctrl Pts',(-1.67442402322111,-1.08498670633101,91.502305956993));
#8803=CARTESIAN_POINT('Ctrl Pts',(-1.65016502050455,-1.12070645916012,91.505079344738));
#8804=CARTESIAN_POINT('Ctrl Pts',(-1.61120871825323,-1.178066998825,91.5095329874751));
#8805=CARTESIAN_POINT('Ctrl Pts',(-1.56918069144311,-1.23350778322811,91.5139866302121));
#8806=CARTESIAN_POINT('Ctrl Pts',(-1.52429668529752,-1.28668068210065,91.5184402729491));
#8807=CARTESIAN_POINT('Ctrl Pts',(-1.47948026045186,-1.33977351918871,91.5228872098906));
#8808=CARTESIAN_POINT('Ctrl Pts',(-1.43181670431929,-1.39060487695719,91.5273341468322));
#8809=CARTESIAN_POINT('Ctrl Pts',(-1.38156468533898,-1.43885599791091,91.5317810837737));
#8810=CARTESIAN_POINT('Ctrl Pts',(-1.33137204957049,-1.48705010012997,91.5362227657344));
#8811=CARTESIAN_POINT('Ctrl Pts',(-1.27859737758551,-1.53266968386654,91.540664447695));
#8812=CARTESIAN_POINT('Ctrl Pts',(-1.22353800024705,-1.57543083772391,91.5451061296557));
#8813=CARTESIAN_POINT('Ctrl Pts',(-1.16851345644702,-1.61816493856382,91.5495450015682));
#8814=CARTESIAN_POINT('Ctrl Pts',(-1.11120746048929,-1.65804389727924,91.5539838734808));
#8815=CARTESIAN_POINT('Ctrl Pts',(-1.05195126414642,-1.69482332423198,91.5584227453934));
#8816=CARTESIAN_POINT('Ctrl Pts',(-0.992712410512399,-1.73159198682702,
91.5628603181664));
#8817=CARTESIAN_POINT('Ctrl Pts',(-0.931524905373209,-1.76526266036815,
91.5672978909395));
#8818=CARTESIAN_POINT('Ctrl Pts',(-0.868748401194261,-1.7956346448881,91.5717354637126));
#8819=CARTESIAN_POINT('Ctrl Pts',(-0.80596892783183,-1.82600806593269,91.5761732463726));
#8820=CARTESIAN_POINT('Ctrl Pts',(-0.741600748042559,-1.85308227707946,
91.5806110290327));
#8821=CARTESIAN_POINT('Ctrl Pts',(-0.676025878173996,-1.87670364590126,
91.5850488116927));
#8822=CARTESIAN_POINT('Ctrl Pts',(-0.610381473243961,-1.90035006263144,
91.5894913001415));
#8823=CARTESIAN_POINT('Ctrl Pts',(-0.543528285864839,-1.92053616273836,
91.5939337885904));
#8824=CARTESIAN_POINT('Ctrl Pts',(-0.475865064633682,-1.937157712413,91.5983762770393));
#8825=CARTESIAN_POINT('Ctrl Pts',(-0.408162420292586,-1.95378894642085,
91.6028213538471));
#8826=CARTESIAN_POINT('Ctrl Pts',(-0.339649283885739,-1.96685140454597,
91.607266430655));
#8827=CARTESIAN_POINT('Ctrl Pts',(-0.270733451114978,-1.97629222559503,
91.6117115074629));
#8828=CARTESIAN_POINT('Ctrl Pts',(-0.201696956710912,-1.98574957615323,
91.616164366956));
#8829=CARTESIAN_POINT('Ctrl Pts',(-0.132256846416913,-1.99157259079294,
91.620617226449));
#8830=CARTESIAN_POINT('Ctrl Pts',(-0.0628240830250762,-1.99376044124967,
91.625070085942));
#8831=CARTESIAN_POINT('Ctrl Pts',(-0.0250067825285576,-1.99495207750497,
91.6274953837019));
#8832=CARTESIAN_POINT('Ctrl Pts',(0.0128083646673936,-1.99506623435737,
91.6299206814618));
#8833=CARTESIAN_POINT('Ctrl Pts',(0.0505556209234334,-1.99410924768255,
91.6323459792217));
#8834=CARTESIAN_POINT('Ctrl Pts',(0.11987161759915,-1.99235191505098,91.6367995991172));
#8835=CARTESIAN_POINT('Ctrl Pts',(0.189233471968186,-1.98697260991991,91.6412532190127));
#8836=CARTESIAN_POINT('Ctrl Pts',(0.258231680319318,-1.97796460073973,91.6457068389081));
#8837=CARTESIAN_POINT('Ctrl Pts',(0.327126019380643,-1.96897015213653,91.6501537543638));
#8838=CARTESIAN_POINT('Ctrl Pts',(0.395657317348736,-1.95635790420461,91.6546006698195));
#8839=CARTESIAN_POINT('Ctrl Pts',(0.463417572739169,-1.94017311489891,91.6590475852751));
#8840=CARTESIAN_POINT('Ctrl Pts',(0.531097787415514,-1.9240074436158,91.6634892478833));
#8841=CARTESIAN_POINT('Ctrl Pts',(0.598008294462548,-1.90427772557105,91.6679309104914));
#8842=CARTESIAN_POINT('Ctrl Pts',(0.663749502519618,-1.88108058317685,91.6723725730996));
#8843=CARTESIAN_POINT('Ctrl Pts',(0.729449138692732,-1.85789810964774,91.6768114269933));
#8844=CARTESIAN_POINT('Ctrl Pts',(0.793980481995075,-1.83125272398766,91.681250280887));
#8845=CARTESIAN_POINT('Ctrl Pts',(0.856958848403317,-1.80129095224599,91.6856891347806));
#8846=CARTESIAN_POINT('Ctrl Pts',(0.919918802009486,-1.7713379403405,91.6901266908995));
#8847=CARTESIAN_POINT('Ctrl Pts',(0.981326238091841,-1.73807067739306,91.6945642470184));
#8848=CARTESIAN_POINT('Ctrl Pts',(1.04081787082229,-1.70168320267815,91.6990018031372));
#8849=CARTESIAN_POINT('Ctrl Pts',(1.10031233611009,-1.66529399545726,91.7034395705401));
#8850=CARTESIAN_POINT('Ctrl Pts',(1.1578904004571,-1.62578453904915,91.707877337943));
#8851=CARTESIAN_POINT('Ctrl Pts',(1.21321628176691,-1.58339313379706,91.7123151053459));
#8852=CARTESIAN_POINT('Ctrl Pts',(1.2686008584175,-1.54095675541633,91.7167575807854));
#8853=CARTESIAN_POINT('Ctrl Pts',(1.32172809347337,-1.495632623975,91.7212000562248));
#8854=CARTESIAN_POINT('Ctrl Pts',(1.37229471426436,-1.44769982375564,91.7256425316642));
#8855=CARTESIAN_POINT('Ctrl Pts',(1.42289081142372,-1.39973908247844,91.7300875967179));
#8856=CARTESIAN_POINT('Ctrl Pts',(1.47092298606983,-1.34916700091813,91.7345326617716));
#8857=CARTESIAN_POINT('Ctrl Pts',(1.51612629089565,-1.29629804927532,91.7389777268253));
#8858=CARTESIAN_POINT('Ctrl Pts',(1.5614087618025,-1.2433365064442,91.7434305766722));
#8859=CARTESIAN_POINT('Ctrl Pts',(1.60385217481339,-1.18807045192681,91.7478834265191));
#8860=CARTESIAN_POINT('Ctrl Pts',(1.64323364245756,-1.13084515243939,91.7523362763659));
#8861=CARTESIAN_POINT('Ctrl Pts',(1.66468453745377,-1.09967480852222,91.7547617221457));
#8862=CARTESIAN_POINT('Ctrl Pts',(1.6852277561755,-1.06792364144393,91.7571871679255));
#8863=CARTESIAN_POINT('Ctrl Pts',(1.70483308141496,-1.0356503884097,91.7596126137053));
#8864=CARTESIAN_POINT('Ctrl Pts',(1.74083141177058,-0.976391834410417,91.7640660975101));
#8865=CARTESIAN_POINT('Ctrl Pts',(1.77380789984148,-0.915136424797846,91.7685195813148));
#8866=CARTESIAN_POINT('Ctrl Pts',(1.80353546187275,-0.852224970455246,91.7729730651195));
#8867=CARTESIAN_POINT('Ctrl Pts',(1.83321825272986,-0.789408263864797,91.7774198417581));
#8868=CARTESIAN_POINT('Ctrl Pts',(1.85966162140974,-0.724940901765582,91.7818666183966));
#8869=CARTESIAN_POINT('Ctrl Pts',(1.88268302922411,-0.659190544510101,91.7863133950352));
#8870=CARTESIAN_POINT('Ctrl Pts',(1.90567722507073,-0.593517906072535,91.7907549154555));
#8871=CARTESIAN_POINT('Ctrl Pts',(1.92525733253197,-0.526565744437922,91.7951964358759));
#8872=CARTESIAN_POINT('Ctrl Pts',(1.9412885679162,-0.458722419964247,91.7996379562963));
#8873=CARTESIAN_POINT('Ctrl Pts',(1.95730965827062,-0.390922028710185,91.8040766659939));
#8874=CARTESIAN_POINT('Ctrl Pts',(1.96978621934225,-0.32223206882486,91.8085153756916));
#8875=CARTESIAN_POINT('Ctrl Pts',(1.97863350693547,-0.253055345195932,91.8129540853892));
#8876=CARTESIAN_POINT('Ctrl Pts',(1.98747820421534,-0.18389887516327,91.8173914955192));
#8877=CARTESIAN_POINT('Ctrl Pts',(1.99269567527279,-0.114256409796314,91.8218289056492));
#8878=CARTESIAN_POINT('Ctrl Pts',(1.99425271452269,-0.0445384454026968,
91.8262663157792));
#8879=CARTESIAN_POINT('Ctrl Pts',(1.99580982735564,0.0251828137443127,91.8307039356137));
#8880=CARTESIAN_POINT('Ctrl Pts',(1.99370615638435,0.0949790893618926,91.8351415554482));
#8881=CARTESIAN_POINT('Ctrl Pts',(1.98796060036666,0.164439088691927,91.8395791752827));
#8882=CARTESIAN_POINT('Ctrl Pts',(1.98220895047904,0.233972758907779,91.8440215017597));
#8883=CARTESIAN_POINT('Ctrl Pts',(1.97280774618898,0.303168951922588,91.8484638282367));
#8884=CARTESIAN_POINT('Ctrl Pts',(1.9598277722544,0.371621669982216,91.8529061547137));
#8885=CARTESIAN_POINT('Ctrl Pts',(1.94684023472766,0.440114276291528,91.8573510697895));
#8886=CARTESIAN_POINT('Ctrl Pts',(1.93026989321702,0.507862069508077,91.8617959848654));
#8887=CARTESIAN_POINT('Ctrl Pts',(1.91023802225024,0.574472158463305,91.8662408999412));
#8888=CARTESIAN_POINT('Ctrl Pts',(1.89017106752955,0.641198908112534,91.8706935998269));
#8889=CARTESIAN_POINT('Ctrl Pts',(1.86663064671297,0.706783515007433,91.8751462997126));
#8890=CARTESIAN_POINT('Ctrl Pts',(1.8397866825987,0.770851817817454,91.8795989995984));
#8891=CARTESIAN_POINT('Ctrl Pts',(1.82515655279538,0.805769447061747,91.8820257491286));
#8892=CARTESIAN_POINT('Ctrl Pts',(1.80954598416172,0.840237088275283,91.8844524986588));
#8893=CARTESIAN_POINT('Ctrl Pts',(1.79298810575163,0.874197469187127,91.886879248189));
#8894=CARTESIAN_POINT('Ctrl Pts',(1.76260114926658,0.936521433128998,91.8913328098439));
#8895=CARTESIAN_POINT('Ctrl Pts',(1.72890042286844,0.99738289868493,91.8957863714989));
#8896=CARTESIAN_POINT('Ctrl Pts',(1.69204986404861,1.05640656002937,91.9002399331538));
#8897=CARTESIAN_POINT('Ctrl Pts',(1.65525479373849,1.11534134524517,91.904686788764));
#8898=CARTESIAN_POINT('Ctrl Pts',(1.61531956165861,1.17244340664813,91.9091336443741));
#8899=CARTESIAN_POINT('Ctrl Pts',(1.5724547756546,1.22736039573592,91.9135804999842));
#8900=CARTESIAN_POINT('Ctrl Pts',(1.52964064386472,1.28221248826913,91.9180221006521));
#8901=CARTESIAN_POINT('Ctrl Pts',(1.48390413373731,1.33488425276784,91.9224637013199));
#8902=CARTESIAN_POINT('Ctrl Pts',(1.43549908588095,1.3850523228149,91.9269053019878));
#8903=CARTESIAN_POINT('Ctrl Pts',(1.38712466146663,1.43518865404436,91.931344092678));
#8904=CARTESIAN_POINT('Ctrl Pts',(1.33608538760082,1.48282408142388,91.9357828833683));
#8905=CARTESIAN_POINT('Ctrl Pts',(1.28267431049402,1.52766952437322,91.9402216740585));
#8906=CARTESIAN_POINT('Ctrl Pts',(1.22927886332582,1.57250184398638,91.9446591658042));
#8907=CARTESIAN_POINT('Ctrl Pts',(1.17351336556581,1.61454548519606,91.9490966575499));
#8908=CARTESIAN_POINT('Ctrl Pts',(1.11570519872292,1.6535505653117,91.9535341492957));
#8909=CARTESIAN_POINT('Ctrl Pts',(1.05789429347484,1.69255749311981,91.9579718512478));
#8910=CARTESIAN_POINT('Ctrl Pts',(0.998040934293289,1.72852530214157,91.9624095532));
#8911=CARTESIAN_POINT('Ctrl Pts',(0.936501343751632,1.76124751118387,91.9668472551522));
#8912=CARTESIAN_POINT('Ctrl Pts',(0.874896481356214,1.79400442697714,91.9712896639448));
#8913=CARTESIAN_POINT('Ctrl Pts',(0.811602251029684,1.82350864138877,91.9757320727375));
#8914=CARTESIAN_POINT('Ctrl Pts',(0.746998474200789,1.84960018437545,91.9801744815301));
#8915=CARTESIAN_POINT('Ctrl Pts',(0.682357049206668,1.87570693233573,91.984619479158));
#8916=CARTESIAN_POINT('Ctrl Pts',(0.616405021962518,1.89839689113825,91.989064476786));
#8917=CARTESIAN_POINT('Ctrl Pts',(0.549538486765532,1.91755965071845,91.9935094744139));
#8918=CARTESIAN_POINT('Ctrl Pts',(0.482554851703556,1.936755969037,91.9979622563337));
#8919=CARTESIAN_POINT('Ctrl Pts',(0.414653988835545,1.95241264749731,92.0024150382534));
#8920=CARTESIAN_POINT('Ctrl Pts',(0.346242539320402,1.96447032720399,92.0068678201732));
#8921=CARTESIAN_POINT('Ctrl Pts',(0.308969750142853,1.97103974441212,92.0092938410063));
#8922=CARTESIAN_POINT('Ctrl Pts',(0.271545501069042,1.97654173171664,92.0117198618395));
#8923=CARTESIAN_POINT('Ctrl Pts',(0.234035822213164,1.98097319427119,92.0141458826726));
#8924=CARTESIAN_POINT('Ctrl Pts',(0.165177654838381,1.9891082250047,92.0185994358268));
#8925=CARTESIAN_POINT('Ctrl Pts',(0.0957580885741036,1.99366488905668,92.0230529889811));
#8926=CARTESIAN_POINT('Ctrl Pts',(0.0261814775965268,1.99457817413378,92.0275065421353));
#8927=CARTESIAN_POINT('Ctrl Pts',(-0.0432903677013928,1.99549008402272,
92.0319533893072));
#8928=CARTESIAN_POINT('Ctrl Pts',(-0.112918302742501,1.99276949691071,92.0364002364791));
#8929=CARTESIAN_POINT('Ctrl Pts',(-0.182292051846247,1.98640307348073,92.040847083651));
#8930=CARTESIAN_POINT('Ctrl Pts',(-0.251583822506288,1.980044173206,92.0452886760167));
#8931=CARTESIAN_POINT('Ctrl Pts',(-0.320621518521699,1.97004803782135,92.0497302683824));
#8932=CARTESIAN_POINT('Ctrl Pts',(-0.388995869555428,1.95645336667369,92.054171860748));
#8933=CARTESIAN_POINT('Ctrl Pts',(-0.457326964862402,1.94286729593498,92.0586106432251));
#8934=CARTESIAN_POINT('Ctrl Pts',(-0.524995068504795,1.92568730078927,92.0630494257022));
#8935=CARTESIAN_POINT('Ctrl Pts',(-0.59159855460696,1.90500359912703,92.0674882081793));
#8936=CARTESIAN_POINT('Ctrl Pts',(-0.658182551705164,1.88432594977178,92.0719256918138));
#8937=CARTESIAN_POINT('Ctrl Pts',(-0.723702082251926,1.86014677425824,92.0763631754483));
#8938=CARTESIAN_POINT('Ctrl Pts',(-0.78776993029633,1.83260636783269,92.0808006590827));
#8939=CARTESIAN_POINT('Ctrl Pts',(-0.851840814932851,1.8050646560881,92.0852383530384));
#8940=CARTESIAN_POINT('Ctrl Pts',(-0.914459431517329,1.77416159271583,92.089676046994));
#8941=CARTESIAN_POINT('Ctrl Pts',(-0.97525948086811,1.74008520121196,92.0941137409497));
#8942=CARTESIAN_POINT('Ctrl Pts',(-1.03612402096819,1.70597266480286,92.0985561419773));
#8943=CARTESIAN_POINT('Ctrl Pts',(-1.0951657156417,1.6686803217795,92.102998543005));
#8944=CARTESIAN_POINT('Ctrl Pts',(-1.15204463276392,1.62844119532141,92.1074409440326));
#8945=CARTESIAN_POINT('Ctrl Pts',(-1.20895669794112,1.58817861819228,92.1118859340152));
#8946=CARTESIAN_POINT('Ctrl Pts',(-1.26370309232811,1.54496614297382,92.1163309239978));
#8947=CARTESIAN_POINT('Ctrl Pts',(-1.31597677668335,1.4990772781048,92.1207759139804));
#8948=CARTESIAN_POINT('Ctrl Pts',(-1.36834200855585,1.45310804752787,92.1252286885261));
#8949=CARTESIAN_POINT('Ctrl Pts',(-1.41822553528151,1.40445341256117,92.1296814630718));
#8950=CARTESIAN_POINT('Ctrl Pts',(-1.46535756086145,1.35342335628073,92.1341342376176));
#8951=CARTESIAN_POINT('Ctrl Pts',(-1.49103743407814,1.32561964194004,92.1365603307971));
#8952=CARTESIAN_POINT('Ctrl Pts',(-1.5159011992894,1.29711133444319,92.1389864239766));
#8953=CARTESIAN_POINT('Ctrl Pts',(-1.53991054849781,1.26795231184976,92.1414125171562));
#8954=CARTESIAN_POINT('Ctrl Pts',(-1.58523602325096,1.21290514955846,92.1459925590475));
#8955=CARTESIAN_POINT('Ctrl Pts',(-1.62770503759097,1.15530429146085,92.1505726009388));
#8956=CARTESIAN_POINT('Ctrl Pts',(-1.66701720851066,1.09548217193587,92.1551526428301));
#8957=CARTESIAN_POINT('Ctrl Pts',(-1.66796412351456,1.09611534438494,91.3549851603904));
#8958=CARTESIAN_POINT('Ctrl Pts',(-1.73430967354358,0.997308734995318,91.3625943436784));
#8959=CARTESIAN_POINT('Ctrl Pts',(-1.92014308949855,0.657612230849117,91.3873052709542));
#8960=CARTESIAN_POINT('Ctrl Pts',(-1.99323138819231,0.269843683907433,91.41201619823));
#8961=CARTESIAN_POINT('Ctrl Pts',(-1.99200409659199,0.00103412633720044,
91.4291179422178));
#8962=CARTESIAN_POINT('Ctrl Pts',(-1.66701720873947,1.09548217158769,91.1951011757363));
#8963=CARTESIAN_POINT('Ctrl Pts',(-1.67557932382123,1.08245302921121,91.1960977547751));
#8964=CARTESIAN_POINT('Ctrl Pts',(-1.68398835949459,1.06932400742616,91.1971000459174));
#8965=CARTESIAN_POINT('Ctrl Pts',(-1.71202140507325,1.02440514260801,91.200523546742));
#8966=CARTESIAN_POINT('Ctrl Pts',(-1.73090480249588,0.992165027452247,91.2029713836732));
#8967=CARTESIAN_POINT('Ctrl Pts',(-1.80883185370803,0.850115668057356,91.2137229628638));
#8968=CARTESIAN_POINT('Ctrl Pts',(-1.8584060144973,0.735450833854669,91.2223409935215));
#8969=CARTESIAN_POINT('Ctrl Pts',(-1.92088412850732,0.543341151059053,91.2364362574407));
#8970=CARTESIAN_POINT('Ctrl Pts',(-1.94051494292932,0.468420806961051,91.2418474567661));
#8971=CARTESIAN_POINT('Ctrl Pts',(-1.96182119974608,0.362269017879838,91.2492658810048));
#8972=CARTESIAN_POINT('Ctrl Pts',(-1.96719483880068,0.331852256753587,91.2513631997857));
#8973=CARTESIAN_POINT('Ctrl Pts',(-1.97550007184297,0.277502475802883,91.2550472633365));
#8974=CARTESIAN_POINT('Ctrl Pts',(-1.97870819664382,0.253618127637724,91.2566445985615));
#8975=CARTESIAN_POINT('Ctrl Pts',(-1.98312730478675,0.215493882486985,91.2591538310612));
#8976=CARTESIAN_POINT('Ctrl Pts',(-1.98461936074998,0.201289701017723,91.2600798094895));
#8977=CARTESIAN_POINT('Ctrl Pts',(-1.9872974410768,0.172858891701633,91.2619138148298));
#8978=CARTESIAN_POINT('Ctrl Pts',(-1.98848355629581,0.158633185401096,91.2628217483202));
#8979=CARTESIAN_POINT('Ctrl Pts',(-1.99128281501323,0.120064314340272,91.2652599793522));
#8980=CARTESIAN_POINT('Ctrl Pts',(-1.99260233042405,0.0957014522708389,
91.2667749776096));
#8981=CARTESIAN_POINT('Ctrl Pts',(-1.99812378007248,-0.0586309298590655,
91.2762476823262));
#8982=CARTESIAN_POINT('Ctrl Pts',(-1.99005564969632,-0.18874000020035,91.2836908192202));
#8983=CARTESIAN_POINT('Ctrl Pts',(-1.95303024900074,-0.418653261848093,
91.2972026299974));
#8984=CARTESIAN_POINT('Ctrl Pts',(-1.92886302470222,-0.518731382220453,
91.3032105393503));
#8985=CARTESIAN_POINT('Ctrl Pts',(-1.88578229316025,-0.651300216300443,
91.3116770229581));
#8986=CARTESIAN_POINT('Ctrl Pts',(-1.87351692648273,-0.685784874258854,
91.3139267886881));
#8987=CARTESIAN_POINT('Ctrl Pts',(-1.85156051344161,-0.742522086628909,
91.3177193875796));
#8988=CARTESIAN_POINT('Ctrl Pts',(-1.84239923379764,-0.764970825290077,
91.3192442299543));
#8989=CARTESIAN_POINT('Ctrl Pts',(-1.82324045126845,-0.809575443542693,
91.3223258433804));
#8990=CARTESIAN_POINT('Ctrl Pts',(-1.81324263369408,-0.831726641397818,
91.3238824176842));
#8991=CARTESIAN_POINT('Ctrl Pts',(-1.78704724524203,-0.887046763279057,
91.3278388273612));
#8992=CARTESIAN_POINT('Ctrl Pts',(-1.77032966423661,-0.9199578218795,91.3302564715431));
#8993=CARTESIAN_POINT('Ctrl Pts',(-1.69014280363983,-1.06752877731028,91.3413980861344));
#8994=CARTESIAN_POINT('Ctrl Pts',(-1.61639067780149,-1.17621073636466,91.3504799246466));
#8995=CARTESIAN_POINT('Ctrl Pts',(-1.48533658335459,-1.33350619318615,91.3647790548516));
#8996=CARTESIAN_POINT('Ctrl Pts',(-1.43503571289753,-1.38749302950276,91.3699321377992));
#8997=CARTESIAN_POINT('Ctrl Pts',(-1.36020150826005,-1.45937702748069,91.3770386660267));
#8998=CARTESIAN_POINT('Ctrl Pts',(-1.33807524244018,-1.479690602599,91.3790770660678));
#8999=CARTESIAN_POINT('Ctrl Pts',(-1.29778321330738,-1.51503848432675,91.3826668924804));
#9000=CARTESIAN_POINT('Ctrl Pts',(-1.27979382724325,-1.53026492983871,91.3842283645877));
#9001=CARTESIAN_POINT('Ctrl Pts',(-1.25062584040304,-1.55407883138959,91.3866894030774));
#9002=CARTESIAN_POINT('Ctrl Pts',(-1.2396191773746,-1.56287246469022,91.387602491826));
#9003=CARTESIAN_POINT('Ctrl Pts',(-1.21718947898448,-1.58040632693127,91.3894303844978));
#9004=CARTESIAN_POINT('Ctrl Pts',(-1.20576335706046,-1.5891410080481,91.3903448528038));
#9005=CARTESIAN_POINT('Ctrl Pts',(-1.17442155760878,-1.61256751174137,91.3928112400276));
#9006=CARTESIAN_POINT('Ctrl Pts',(-1.15432471305096,-1.62701400188971,91.3943474033065));
#9007=CARTESIAN_POINT('Ctrl Pts',(-1.06335128333963,-1.68987522693105,91.4011269088481));
#9008=CARTESIAN_POINT('Ctrl Pts',(-0.989656567701482,-1.73406373054063,
91.4061579598815));
#9009=CARTESIAN_POINT('Ctrl Pts',(-0.779341590488958,-1.84238210631005,
91.4199133512176));
#9010=CARTESIAN_POINT('Ctrl Pts',(-0.637968801043272,-1.89597917343904,
91.4285463309824));
#9011=CARTESIAN_POINT('Ctrl Pts',(-0.458170840760185,-1.94173100152174,
91.4398487481898));
#9012=CARTESIAN_POINT('Ctrl Pts',(-0.424211601296343,-1.94943173564965,
91.4419945967116));
#9013=CARTESIAN_POINT('Ctrl Pts',(-0.366707009382995,-1.96089802155084,
91.4456565615681));
#9014=CARTESIAN_POINT('Ctrl Pts',(-0.343263552849276,-1.96513743427046,
91.4471572598384));
#9015=CARTESIAN_POINT('Ctrl Pts',(-0.295199557599133,-1.97294283568278,
91.4502525870432));
#9016=CARTESIAN_POINT('Ctrl Pts',(-0.27057707998445,-1.97647012688136,91.4518481627151));
#9017=CARTESIAN_POINT('Ctrl Pts',(-0.20680417361142,-1.9843919335312,91.4560088253887));
#9018=CARTESIAN_POINT('Ctrl Pts',(-0.167579586730039,-1.98808853701402,
91.45859526912));
#9019=CARTESIAN_POINT('Ctrl Pts',(-0.0798498535103628,-1.99374174514934,
91.4644440003917));
#9020=CARTESIAN_POINT('Ctrl Pts',(-0.0313318172720462,-1.99509395068248,
91.4677221457275));
#9021=CARTESIAN_POINT('Ctrl Pts',(0.146285484972184,-1.99356375914313,91.479866602198));
#9022=CARTESIAN_POINT('Ctrl Pts',(0.274970381662822,-1.97992003533079,91.4889672513183));
#9023=CARTESIAN_POINT('Ctrl Pts',(0.458664157106047,-1.9421817350225,91.5019290226276));
#9024=CARTESIAN_POINT('Ctrl Pts',(0.515368606921603,-1.92791055064655,91.5059212686355));
#9025=CARTESIAN_POINT('Ctrl Pts',(0.590260402158344,-1.90552066553798,91.5111154396459));
#9026=CARTESIAN_POINT('Ctrl Pts',(0.609068002062043,-1.89959274324658,91.512413005821));
#9027=CARTESIAN_POINT('Ctrl Pts',(0.64058808141338,-1.88914170963453,91.5145724723778));
#9028=CARTESIAN_POINT('Ctrl Pts',(0.653347762670158,-1.88476689092099,91.5154423291691));
#9029=CARTESIAN_POINT('Ctrl Pts',(0.680977099075295,-1.87497949063178,91.5173155890082));
#9030=CARTESIAN_POINT('Ctrl Pts',(0.695828254476938,-1.86951891656941,91.5183162724433));
#9031=CARTESIAN_POINT('Ctrl Pts',(0.740716170149424,-1.85240519567818,91.5213264274254));
#9032=CARTESIAN_POINT('Ctrl Pts',(0.770538384695544,-1.84020007477372,91.5233065124223));
#9033=CARTESIAN_POINT('Ctrl Pts',(0.84273439974789,-1.80858982454666,91.5280818006507));
#9034=CARTESIAN_POINT('Ctrl Pts',(0.884749811014522,-1.78841177850315,91.5308452190301));
#9035=CARTESIAN_POINT('Ctrl Pts',(1.01338409869734,-1.72099069413277,91.5393691118898));
#9036=CARTESIAN_POINT('Ctrl Pts',(1.09723048164694,-1.66878467764027,91.5450240073601));
#9037=CARTESIAN_POINT('Ctrl Pts',(1.19100321263822,-1.60026410688594,91.5518112088524));
#9038=CARTESIAN_POINT('Ctrl Pts',(1.20499748792955,-1.58975309541588,91.5528369049176));
#9039=CARTESIAN_POINT('Ctrl Pts',(1.27540301861102,-1.53540815803632,91.5580695371411));
#9040=CARTESIAN_POINT('Ctrl Pts',(1.32956388383169,-1.48875433638958,91.5623368998203));
#9041=CARTESIAN_POINT('Ctrl Pts',(1.40287307230182,-1.41840933881711,91.5685712564255));
#9042=CARTESIAN_POINT('Ctrl Pts',(1.42416571533331,-1.39702890891455,91.5704420483364));
#9043=CARTESIAN_POINT('Ctrl Pts',(1.4611360939455,-1.35818229293506,91.5738055502104));
#9044=CARTESIAN_POINT('Ctrl Pts',(1.47700616769576,-1.34090660743516,91.5752894895947));
#9045=CARTESIAN_POINT('Ctrl Pts',(1.51011776599451,-1.30356117363778,91.5784750622594));
#9046=CARTESIAN_POINT('Ctrl Pts',(1.52727190598122,-1.28342035729944,91.5801799627468));
#9047=CARTESIAN_POINT('Ctrl Pts',(1.57450070073456,-1.22568056242885,91.5850342685134));
#9048=CARTESIAN_POINT('Ctrl Pts',(1.60362021998845,-1.18732760319835,91.5882206175824));
#9049=CARTESIAN_POINT('Ctrl Pts',(1.66869295526831,-1.09485534537592,91.5958183280696));
#9050=CARTESIAN_POINT('Ctrl Pts',(1.70344531005663,-1.03996021864376,91.6002654464387));
#9051=CARTESIAN_POINT('Ctrl Pts',(1.80143766910359,-0.867040755177769,91.6140296799328));
#9052=CARTESIAN_POINT('Ctrl Pts',(1.85553409605499,-0.744265730251361,91.6234951228334));
#9053=CARTESIAN_POINT('Ctrl Pts',(1.90691360074303,-0.586301970193441,91.6347501663742));
#9054=CARTESIAN_POINT('Ctrl Pts',(1.9161518954768,-0.555366244806632,91.6369110445818));
#9055=CARTESIAN_POINT('Ctrl Pts',(1.92879489433107,-0.508948212035358,91.6400759291906));
#9056=CARTESIAN_POINT('Ctrl Pts',(1.93277226487754,-0.493628847464306,91.6411080225453));
#9057=CARTESIAN_POINT('Ctrl Pts',(1.9397910655852,-0.465208557078174,91.6429977997215));
#9058=CARTESIAN_POINT('Ctrl Pts',(1.94288283164275,-0.452122430712377,91.643858004984));
#9059=CARTESIAN_POINT('Ctrl Pts',(1.95015483795353,-0.419890041959174,91.6459538653473));
#9060=CARTESIAN_POINT('Ctrl Pts',(1.95418568228366,-0.400711777083527,91.6471813526323));
#9061=CARTESIAN_POINT('Ctrl Pts',(1.96980637504549,-0.320538326643491,91.6522433806256));
#9062=CARTESIAN_POINT('Ctrl Pts',(1.9788290634956,-0.259073266478648,91.6559580373196));
#9063=CARTESIAN_POINT('Ctrl Pts',(2.00145621125214,-0.0314083848154977,
91.6694318399111));
#9064=CARTESIAN_POINT('Ctrl Pts',(1.99708636270522,0.135872062533571,91.6788355447133));
#9065=CARTESIAN_POINT('Ctrl Pts',(1.96535082321936,0.344015675837371,91.6915127572879));
#9066=CARTESIAN_POINT('Ctrl Pts',(1.95731360813261,0.387135191941691,91.694188987242));
#9067=CARTESIAN_POINT('Ctrl Pts',(1.94233162261265,0.455009759843278,91.6985019189054));
#9068=CARTESIAN_POINT('Ctrl Pts',(1.93631798078774,0.479956866190553,91.7001088520919));
#9069=CARTESIAN_POINT('Ctrl Pts',(1.92384545518493,0.527640580162321,91.7032257872347));
#9070=CARTESIAN_POINT('Ctrl Pts',(1.91746039507092,0.550392106677105,91.7047331464944));
#9071=CARTESIAN_POINT('Ctrl Pts',(1.90140057654431,0.603941446658325,91.70833126747));
#9072=CARTESIAN_POINT('Ctrl Pts',(1.89137966215194,0.634627602559148,91.710433099684));
#9073=CARTESIAN_POINT('Ctrl Pts',(1.84813443505409,0.756914806522421,91.7189760451027));
#9074=CARTESIAN_POINT('Ctrl Pts',(1.80896765972359,0.846257791933204,91.7256082575551));
#9075=CARTESIAN_POINT('Ctrl Pts',(1.6988699375753,1.05449057473166,91.7419282848842));
#9076=CARTESIAN_POINT('Ctrl Pts',(1.6217926772881,1.16957235055995,91.7517056387603));
#9077=CARTESIAN_POINT('Ctrl Pts',(1.51512467160417,1.29778466611345,91.7629563826147));
#9078=CARTESIAN_POINT('Ctrl Pts',(1.49633444120909,1.31940564194575,91.7648661385844));
#9079=CARTESIAN_POINT('Ctrl Pts',(1.46690557390785,1.35183022826784,91.767739943736));
#9080=CARTESIAN_POINT('Ctrl Pts',(1.45659936098922,1.36292892917057,91.7687254417333));
#9081=CARTESIAN_POINT('Ctrl Pts',(1.43674628162087,1.38382613758694,91.7705826188315));
#9082=CARTESIAN_POINT('Ctrl Pts',(1.42722345728877,1.39364553207016,91.7714557956476));
#9083=CARTESIAN_POINT('Ctrl Pts',(1.4027539968117,1.41836317565158,91.7736572157053));
#9084=CARTESIAN_POINT('Ctrl Pts',(1.38767007498224,1.43312411247091,91.7749752097799));
#9085=CARTESIAN_POINT('Ctrl Pts',(1.30774331981868,1.50889400906135,91.781776874104));
#9086=CARTESIAN_POINT('Ctrl Pts',(1.2390969401349,1.56575732856078,91.7870094347413));
#9087=CARTESIAN_POINT('Ctrl Pts',(1.04025906407855,1.70916921291684,91.8012776334048));
#9088=CARTESIAN_POINT('Ctrl Pts',(0.903374751413852,1.78530348559128,91.810201179693));
#9089=CARTESIAN_POINT('Ctrl Pts',(0.727551598145605,1.85764743259769,91.8217971848367));
#9090=CARTESIAN_POINT('Ctrl Pts',(0.695760828190992,1.86978661044983,91.8238963140656));
#9091=CARTESIAN_POINT('Ctrl Pts',(0.641353599884152,1.88898212410908,91.8275019398981));
#9092=CARTESIAN_POINT('Ctrl Pts',(0.618893038786636,1.89645965782163,91.8289941073558));
#9093=CARTESIAN_POINT('Ctrl Pts',(0.572413408395258,1.91101996362131,91.8320921716486));
#9094=CARTESIAN_POINT('Ctrl Pts',(0.548383493219682,1.91805366473135,91.833699381683));
#9095=CARTESIAN_POINT('Ctrl Pts',(0.485248602099012,1.93525024501677,91.8379390698288));
#9096=CARTESIAN_POINT('Ctrl Pts',(0.445957756683675,1.94468018044857,91.8405945899291));
#9097=CARTESIAN_POINT('Ctrl Pts',(0.299098904158719,1.97524220960155,91.8505880219016));
#9098=CARTESIAN_POINT('Ctrl Pts',(0.190143268837779,1.9886884513686,91.8581494306954));
#9099=CARTESIAN_POINT('Ctrl Pts',(-0.0362804851818633,1.99785038105052,
91.873946809047));
#9100=CARTESIAN_POINT('Ctrl Pts',(-0.153406868461913,1.99228322963201,91.8821631472331));
#9101=CARTESIAN_POINT('Ctrl Pts',(-0.292896635898926,1.97327206342784,91.891590669227));
#9102=CARTESIAN_POINT('Ctrl Pts',(-0.316359794682336,1.96964658642417,91.893163493957));
#9103=CARTESIAN_POINT('Ctrl Pts',(-0.353726227510946,1.96318781038201,91.8956417289748));
#9104=CARTESIAN_POINT('Ctrl Pts',(-0.367673065329059,1.96062366975797,91.8965607596371));
#9105=CARTESIAN_POINT('Ctrl Pts',(-0.395724085708324,1.95515659565229,91.8983955376101));
#9106=CARTESIAN_POINT('Ctrl Pts',(-0.409826494878345,1.95224925161995,91.8993110009162));
#9107=CARTESIAN_POINT('Ctrl Pts',(-0.448154128414568,1.94391401336998,91.9017831335129));
#9108=CARTESIAN_POINT('Ctrl Pts',(-0.472312265026185,1.93818602568922,91.9033239269178));
#9109=CARTESIAN_POINT('Ctrl Pts',(-0.578855065282055,1.91081377302493,91.9100671939426));
#9110=CARTESIAN_POINT('Ctrl Pts',(-0.659917992526919,1.88435494320403,91.9150613237878));
#9111=CARTESIAN_POINT('Ctrl Pts',(-0.879567033286966,1.79674060707064,91.9288133950842));
#9112=CARTESIAN_POINT('Ctrl Pts',(-1.01324101328546,1.72489237665278,91.9374767525121));
#9113=CARTESIAN_POINT('Ctrl Pts',(-1.16600183835751,1.61884850364597,91.9488072208559));
#9114=CARTESIAN_POINT('Ctrl Pts',(-1.19397412660394,1.59832922924135,91.9509453209955));
#9115=CARTESIAN_POINT('Ctrl Pts',(-1.24019268575352,1.56253476575578,91.9545964851102));
#9116=CARTESIAN_POINT('Ctrl Pts',(-1.25872690999296,1.54764313685414,91.9560942743908));
#9117=CARTESIAN_POINT('Ctrl Pts',(-1.2960817404471,1.51651485083386,91.9591854448061));
#9118=CARTESIAN_POINT('Ctrl Pts',(-1.31487381040935,1.50025062588985,91.9607798051385));
#9119=CARTESIAN_POINT('Ctrl Pts',(-1.36266970273427,1.45729616651561,91.9649407316049));
#9120=CARTESIAN_POINT('Ctrl Pts',(-1.39119391208288,1.43009089575,91.9675287552192));
#9121=CARTESIAN_POINT('Ctrl Pts',(-1.45302186770433,1.36752068885605,91.9733819195505));
#9122=CARTESIAN_POINT('Ctrl Pts',(-1.48587676392072,1.33174886184449,91.9766629977819));
#9123=CARTESIAN_POINT('Ctrl Pts',(-1.57140396963382,1.23151974034883,91.9856740456171));
#9124=CARTESIAN_POINT('Ctrl Pts',(-1.62137251005126,1.1649406487014,91.9914720109716));
#9125=CARTESIAN_POINT('Ctrl Pts',(-1.66701737487202,1.09548191878041,91.9972724317));
#9126=CARTESIAN_POINT('Origin',(0.,0.,89.2710285354474));
#9127=CARTESIAN_POINT('',(-1.66701720827313,1.09548217229732,92.9566930507716));
#9128=CARTESIAN_POINT('',(-1.66701723320527,1.09548213435759,92.7986587716037));
#9129=CARTESIAN_POINT('',(-1.66701720851066,1.09548217193587,89.2710285354474));
#9130=CARTESIAN_POINT('',(-1.99474929503159,-0.00167704232401422,92.229118772657));
#9131=CARTESIAN_POINT('Ctrl Pts',(-1.66701720827313,1.09548217229732,92.9566930507716));
#9132=CARTESIAN_POINT('Ctrl Pts',(-1.66512381604442,1.09836338525276,92.9564629794761));
#9133=CARTESIAN_POINT('Ctrl Pts',(-1.66322292902265,1.10123972771993,92.956232653761));
#9134=CARTESIAN_POINT('Ctrl Pts',(-1.63018205132079,1.1509550941144,92.9522405013284));
#9135=CARTESIAN_POINT('Ctrl Pts',(-1.59708453028584,1.19645780862156,92.9484138355263));
#9136=CARTESIAN_POINT('Ctrl Pts',(-1.47970949905464,1.34426358271211,92.9354182963228));
#9137=CARTESIAN_POINT('Ctrl Pts',(-1.38717854340582,1.4395550287022,92.9260494118629));
#9138=CARTESIAN_POINT('Ctrl Pts',(-1.25228112725285,1.55330350242768,92.9139562448849));
#9139=CARTESIAN_POINT('Ctrl Pts',(-1.21774614593903,1.58052355681295,92.9109813844852));
#9140=CARTESIAN_POINT('Ctrl Pts',(-1.16925476596872,1.61620998206909,92.9069958285298));
#9141=CARTESIAN_POINT('Ctrl Pts',(-1.15605453136798,1.6256781279405,92.9059295344719));
#9142=CARTESIAN_POINT('Ctrl Pts',(-1.13174286592118,1.642670280379,92.9040016017614));
#9143=CARTESIAN_POINT('Ctrl Pts',(-1.12066857875206,1.65024529753811,92.9031368139206));
#9144=CARTESIAN_POINT('Ctrl Pts',(-1.09622385579789,1.66660634725702,92.9012578430934));
#9145=CARTESIAN_POINT('Ctrl Pts',(-1.08282289954378,1.67534416390961,92.9002466888766));
#9146=CARTESIAN_POINT('Ctrl Pts',(-1.04125342754282,1.70174148086608,92.897163153061));
#9147=CARTESIAN_POINT('Ctrl Pts',(-1.01274612410691,1.71885960544245,92.8951223607961));
#9148=CARTESIAN_POINT('Ctrl Pts',(-0.84937331862725,1.81148549497801,92.8837597999284));
#9149=CARTESIAN_POINT('Ctrl Pts',(-0.706510164299463,1.87183523764905,92.8750430700305));
#9150=CARTESIAN_POINT('Ctrl Pts',(-0.484671798284654,1.93648402682211,92.8614881239828));
#9151=CARTESIAN_POINT('Ctrl Pts',(-0.410080563385768,1.95364002248051,92.8569342095646));
#9152=CARTESIAN_POINT('Ctrl Pts',(-0.304300620752226,1.97164377598798,92.8503584569659));
#9153=CARTESIAN_POINT('Ctrl Pts',(-0.273793309906842,1.97611110740478,92.8484489675302));
#9154=CARTESIAN_POINT('Ctrl Pts',(-0.21984103025048,1.98273830019026,92.84504252305));
#9155=CARTESIAN_POINT('Ctrl Pts',(-0.196438018131312,1.98519351032647,92.8435552040201));
#9156=CARTESIAN_POINT('Ctrl Pts',(-0.147003864983722,1.98949698004184,92.8403905890866));
#9157=CARTESIAN_POINT('Ctrl Pts',(-0.120969083208511,1.99124954314883,92.8387105532682));
#9158=CARTESIAN_POINT('Ctrl Pts',(-0.0488206744255768,1.99468619157877,
92.8340149021936));
#9159=CARTESIAN_POINT('Ctrl Pts',(-0.00267406652750284,1.99528161792044,
92.8309661733468));
#9160=CARTESIAN_POINT('Ctrl Pts',(0.104374352442575,1.99294938453869,92.8237863606924));
#9161=CARTESIAN_POINT('Ctrl Pts',(0.165202414545443,1.98883090387109,92.8196250521618));
#9162=CARTESIAN_POINT('Ctrl Pts',(0.311617239347066,1.97215425742549,92.8094447888385));
#9163=CARTESIAN_POINT('Ctrl Pts',(0.396764083393373,1.95680229203769,92.8033849086056));
#9164=CARTESIAN_POINT('Ctrl Pts',(0.55326688231232,1.91794749495535,92.7921705483738));
#9165=CARTESIAN_POINT('Ctrl Pts',(0.624825553610229,1.89584333655704,92.7870136502784));
#9166=CARTESIAN_POINT('Ctrl Pts',(0.714411738766203,1.86254483243037,92.7806481481676));
#9167=CARTESIAN_POINT('Ctrl Pts',(0.733732086686501,1.85501878513223,92.779281059553));
#9168=CARTESIAN_POINT('Ctrl Pts',(0.765421092324284,1.84210205798646,92.7770523118576));
#9169=CARTESIAN_POINT('Ctrl Pts',(0.777858340687367,1.83688483205883,92.7761811175238));
#9170=CARTESIAN_POINT('Ctrl Pts',(0.804245992164879,1.82549953327339,92.7743414715752));
#9171=CARTESIAN_POINT('Ctrl Pts',(0.818180149032501,1.81929696350458,92.7733750417506));
#9172=CARTESIAN_POINT('Ctrl Pts',(0.858535479865199,1.80077597720875,92.7705868704248));
#9173=CARTESIAN_POINT('Ctrl Pts',(0.884760519831416,1.78803700051856,92.7687885144857));
#9174=CARTESIAN_POINT('Ctrl Pts',(1.04928675523246,1.70361061791707,92.7575342037621));
#9175=CARTESIAN_POINT('Ctrl Pts',(1.17908145383222,1.61649908228052,92.7487466732126));
#9176=CARTESIAN_POINT('Ctrl Pts',(1.30244256925268,1.51086549218848,92.7392382788848));
#9177=CARTESIAN_POINT('Ctrl Pts',(1.30743777834954,1.50654493350637,92.7388511491093));
#9178=CARTESIAN_POINT('Ctrl Pts',(1.36919806408038,1.45258745639231,92.7340375230737));
#9179=CARTESIAN_POINT('Ctrl Pts',(1.42312077808083,1.39979971139823,92.7295448296975));
#9180=CARTESIAN_POINT('Ctrl Pts',(1.49461554727972,1.32139888167711,92.7230409700689));
#9181=CARTESIAN_POINT('Ctrl Pts',(1.5147803578578,1.29823377942307,92.7211385771524));
#9182=CARTESIAN_POINT('Ctrl Pts',(1.54942762486827,1.25652480124698,92.7177401249473));
#9183=CARTESIAN_POINT('Ctrl Pts',(1.56413206052924,1.23817258933805,92.7162535445554));
#9184=CARTESIAN_POINT('Ctrl Pts',(1.59449774242884,1.19886967185534,92.7130855916059));
#9185=CARTESIAN_POINT('Ctrl Pts',(1.61007812152772,1.17786241759925,92.7114013877577));
#9186=CARTESIAN_POINT('Ctrl Pts',(1.65218763174429,1.11868837558988,92.7066790831089));
#9187=CARTESIAN_POINT('Ctrl Pts',(1.67780118160053,1.07989363333188,92.7036072340099));
#9188=CARTESIAN_POINT('Ctrl Pts',(1.73416025946046,0.98767942711209,92.6963578677965));
#9189=CARTESIAN_POINT('Ctrl Pts',(1.76383083329037,0.933660627355826,92.6921492376621));
#9190=CARTESIAN_POINT('Ctrl Pts',(1.82900780333406,0.800766437993345,92.6819193565281));
#9191=CARTESIAN_POINT('Ctrl Pts',(1.86197932191981,0.720783405219669,92.675859132894));
#9192=CARTESIAN_POINT('Ctrl Pts',(1.91326597479264,0.569098332921683,92.6647268650887));
#9193=CARTESIAN_POINT('Ctrl Pts',(1.93298742561041,0.498017310291534,92.6596502928297));
#9194=CARTESIAN_POINT('Ctrl Pts',(1.95314709962975,0.405797596330233,92.6533638192294));
#9195=CARTESIAN_POINT('Ctrl Pts',(1.95724958197575,0.38552488663339,92.6520002019566));
#9196=CARTESIAN_POINT('Ctrl Pts',(1.96350373150585,0.35194078766674,92.6497754400328));
#9197=CARTESIAN_POINT('Ctrl Pts',(1.96583700966981,0.338665198776039,92.6489048300368));
#9198=CARTESIAN_POINT('Ctrl Pts',(1.97052669084244,0.310298805258759,92.6470645062734));
#9199=CARTESIAN_POINT('Ctrl Pts',(1.97284466174229,0.295202920754279,92.6460968480187));
#9200=CARTESIAN_POINT('Ctrl Pts',(1.97909725818879,0.251112834248299,92.6433008190052));
#9201=CARTESIAN_POINT('Ctrl Pts',(1.98256779897893,0.222055713174705,92.6414960369726));
#9202=CARTESIAN_POINT('Ctrl Pts',(1.99865029732456,0.056555362018515,92.6313780426267));
#9203=CARTESIAN_POINT('Ctrl Pts',(1.99781750710646,-0.0808364886002574,
92.6235797722326));
#9204=CARTESIAN_POINT('Ctrl Pts',(1.97235127928098,-0.313467754021576,92.6099561622677));
#9205=CARTESIAN_POINT('Ctrl Pts',(1.95478429833044,-0.408958465645835,92.6042431871923));
#9206=CARTESIAN_POINT('Ctrl Pts',(1.92215941976946,-0.534214770727629,92.5963290008082));
#9207=CARTESIAN_POINT('Ctrl Pts',(1.91320778182807,-0.565436161204636,92.594321230139));
#9208=CARTESIAN_POINT('Ctrl Pts',(1.89641966548098,-0.619015767150256,92.5908068167942));
#9209=CARTESIAN_POINT('Ctrl Pts',(1.88893953976302,-0.641479075489736,92.5893121025613));
#9210=CARTESIAN_POINT('Ctrl Pts',(1.8725357452177,-0.687963560479017,92.586171812602));
#9211=CARTESIAN_POINT('Ctrl Pts',(1.86354551565167,-0.711956450074776,92.5845242336411));
#9212=CARTESIAN_POINT('Ctrl Pts',(1.83803151686993,-0.776250307171098,92.5800337604902));
#9213=CARTESIAN_POINT('Ctrl Pts',(1.82064666239968,-0.816192158622653,92.5771624645826));
#9214=CARTESIAN_POINT('Ctrl Pts',(1.76864290545093,-0.925725573033864,92.5690546812247));
#9215=CARTESIAN_POINT('Ctrl Pts',(1.73124625090235,-0.993906353143329,92.5637337001686));
#9216=CARTESIAN_POINT('Ctrl Pts',(1.61331812442402,-1.18196924372334,92.5483395797541));
#9217=CARTESIAN_POINT('Ctrl Pts',(1.52362577322996,-1.29553621978236,92.5381206207385));
#9218=CARTESIAN_POINT('Ctrl Pts',(1.40622023928125,-1.41495903748831,92.5269162865922));
#9219=CARTESIAN_POINT('Ctrl Pts',(1.38968877526365,-1.43119867908737,92.5253823455063));
#9220=CARTESIAN_POINT('Ctrl Pts',(1.36267266306689,-1.45682827714503,92.5229500419429));
#9221=CARTESIAN_POINT('Ctrl Pts',(1.35236546507571,-1.46640141269237,92.5220388732788));
#9222=CARTESIAN_POINT('Ctrl Pts',(1.33120429780437,-1.48564259021605,92.52020360882));
#9223=CARTESIAN_POINT('Ctrl Pts',(1.32034430846007,-1.495302553684,92.5192800627295));
#9224=CARTESIAN_POINT('Ctrl Pts',(1.29015154525115,-1.52157358064041,92.5167591975319));
#9225=CARTESIAN_POINT('Ctrl Pts',(1.27060384742114,-1.53793471099332,92.5151788294073));
#9226=CARTESIAN_POINT('Ctrl Pts',(1.22473274330075,-1.57485632299711,92.5115734706857));
#9227=CARTESIAN_POINT('Ctrl Pts',(1.19819551642144,-1.59513963810258,92.5095631387166));
#9228=CARTESIAN_POINT('Ctrl Pts',(1.09797276867935,-1.66783016920479,92.5021942735151));
#9229=CARTESIAN_POINT('Ctrl Pts',(1.02125738519878,-1.71587782844855,92.4969836481084));
#9230=CARTESIAN_POINT('Ctrl Pts',(0.847769588897766,-1.80876439191976,92.4855665615558));
#9231=CARTESIAN_POINT('Ctrl Pts',(0.75013898529938,-1.85138607025453,92.4793600471662));
#9232=CARTESIAN_POINT('Ctrl Pts',(0.614566799610138,-1.89807973439372,92.4706530171061));
#9233=CARTESIAN_POINT('Ctrl Pts',(0.579224922797734,-1.9091613994254,92.4683767978636));
#9234=CARTESIAN_POINT('Ctrl Pts',(0.520097644003237,-1.92590822975462,92.4645461644899));
#9235=CARTESIAN_POINT('Ctrl Pts',(0.496479181757247,-1.93213157046368,92.4630102124657));
#9236=CARTESIAN_POINT('Ctrl Pts',(0.449036207356767,-1.94370522938138,92.4599104069859));
#9237=CARTESIAN_POINT('Ctrl Pts',(0.425215900680437,-1.94905486943253,92.4583468333448));
#9238=CARTESIAN_POINT('Ctrl Pts',(0.36508809144613,-1.96140388089001,92.4543794346653));
#9239=CARTESIAN_POINT('Ctrl Pts',(0.328674292161789,-1.96783317525256,92.4519579230179));
#9240=CARTESIAN_POINT('Ctrl Pts',(0.18823846661758,-1.98862225337355,92.4425416943105));
#9241=CARTESIAN_POINT('Ctrl Pts',(0.0833340461069003,-1.99577109174912,
92.4353344691009));
#9242=CARTESIAN_POINT('Ctrl Pts',(-0.153055666163285,-1.99320737284861,
92.4188830011419));
#9243=CARTESIAN_POINT('Ctrl Pts',(-0.284022896300073,-1.97879678781788,
92.4096160131897));
#9244=CARTESIAN_POINT('Ctrl Pts',(-0.434377101032974,-1.94700753477385,
92.399351377401));
#9245=CARTESIAN_POINT('Ctrl Pts',(-0.456050581643854,-1.94204525526638,
92.3978817343252));
#9246=CARTESIAN_POINT('Ctrl Pts',(-0.489792026253793,-1.9337238810199,92.3956141841978));
#9247=CARTESIAN_POINT('Ctrl Pts',(-0.501918349230599,-1.93061188979822,
92.3948034074975));
#9248=CARTESIAN_POINT('Ctrl Pts',(-0.527836765331375,-1.92369970137956,
92.3930805982362));
#9249=CARTESIAN_POINT('Ctrl Pts',(-0.54161901417274,-1.9198648561112,92.3921706603953));
#9250=CARTESIAN_POINT('Ctrl Pts',(-0.578754295923217,-1.90910040108312,
92.3897326495691));
#9251=CARTESIAN_POINT('Ctrl Pts',(-0.602024335072754,-1.90189055984074,
92.3882197132617));
#9252=CARTESIAN_POINT('Ctrl Pts',(-0.702192348769968,-1.86883230099175,
92.3817480125527));
#9253=CARTESIAN_POINT('Ctrl Pts',(-0.777612256578105,-1.83873053833885,
92.3769787560407));
#9254=CARTESIAN_POINT('Ctrl Pts',(-0.994343385309559,-1.73649920003214,
92.3630263379002));
#9255=CARTESIAN_POINT('Ctrl Pts',(-1.12910886947991,-1.65204649319573,92.3539746838506));
#9256=CARTESIAN_POINT('Ctrl Pts',(-1.27867455853763,-1.53138940789677,92.3422478967131));
#9257=CARTESIAN_POINT('Ctrl Pts',(-1.30434970509759,-1.50958066520973,92.3401689376513));
#9258=CARTESIAN_POINT('Ctrl Pts',(-1.34706822140963,-1.4713913997486,92.3365867774337));
#9259=CARTESIAN_POINT('Ctrl Pts',(-1.36439550319081,-1.45533854398623,92.3350974252666));
#9260=CARTESIAN_POINT('Ctrl Pts',(-1.39956898576976,-1.42157175559462,92.331995182526));
#9261=CARTESIAN_POINT('Ctrl Pts',(-1.41737339220613,-1.40382056297502,92.3303807974477));
#9262=CARTESIAN_POINT('Ctrl Pts',(-1.46328595469061,-1.35628125464582,92.3260970787846));
#9263=CARTESIAN_POINT('Ctrl Pts',(-1.4908192484125,-1.32595708371911,92.3234037911163));
#9264=CARTESIAN_POINT('Ctrl Pts',(-1.57768093285815,-1.22416308561304,92.3144827358484));
#9265=CARTESIAN_POINT('Ctrl Pts',(-1.63294954215236,-1.14940182351029,92.3081079748186));
#9266=CARTESIAN_POINT('Ctrl Pts',(-1.75130124523737,-0.96345454898082,92.2927825172896));
#9267=CARTESIAN_POINT('Ctrl Pts',(-1.80931854440083,-0.849511601192616,
92.2837850095712));
#9268=CARTESIAN_POINT('Ctrl Pts',(-1.86582911150276,-0.705989065833395,
92.2734085102));
#9269=CARTESIAN_POINT('Ctrl Pts',(-1.87510184208267,-0.680978765927614,
92.2716344290136));
#9270=CARTESIAN_POINT('Ctrl Pts',(-1.88872639309898,-0.641839795069339,
92.2689187658891));
#9271=CARTESIAN_POINT('Ctrl Pts',(-1.89342719833468,-0.627836912269911,
92.2679590579857));
#9272=CARTESIAN_POINT('Ctrl Pts',(-1.90224836965651,-0.600559601880096,
92.2661143122533));
#9273=CARTESIAN_POINT('Ctrl Pts',(-1.90638628842404,-0.587292115015154,
92.2652284298843));
#9274=CARTESIAN_POINT('Ctrl Pts',(-1.91680040188146,-0.55263081355425,92.2629411117079));
#9275=CARTESIAN_POINT('Ctrl Pts',(-1.92285741684199,-0.53117233542612,92.2615516560956));
#9276=CARTESIAN_POINT('Ctrl Pts',(-1.95473128816408,-0.410551123424886,
92.2538661210989));
#9277=CARTESIAN_POINT('Ctrl Pts',(-1.97324006091968,-0.309604766890619,
92.2478981624538));
#9278=CARTESIAN_POINT('Ctrl Pts',(-1.99107547179722,-0.139222425586477,
92.237957398685));
#9279=CARTESIAN_POINT('Ctrl Pts',(-1.99469315035772,-0.0704487531436606,
92.2339810148349));
#9280=CARTESIAN_POINT('Ctrl Pts',(-1.99474933524002,-0.00162851450148592,
92.2299465820693));
#9281=CARTESIAN_POINT('Ctrl Pts',(-1.66701720851066,1.09548217193587,92.1551526428301));
#9282=CARTESIAN_POINT('Ctrl Pts',(-1.70501540924007,1.03765954722219,92.1595796013792));
#9283=CARTESIAN_POINT('Ctrl Pts',(-1.74006413474923,0.977762240127359,92.1640065599282));
#9284=CARTESIAN_POINT('Ctrl Pts',(-1.77193162675481,0.916125467720477,92.1684335184773));
#9285=CARTESIAN_POINT('Ctrl Pts',(-1.80376472481447,0.854555218647657,92.1728556990987));
#9286=CARTESIAN_POINT('Ctrl Pts',(-1.83242317544167,0.791249665360261,92.17727787972));
#9287=CARTESIAN_POINT('Ctrl Pts',(-1.85771941210735,0.726571502592491,92.1817000603414));
#9288=CARTESIAN_POINT('Ctrl Pts',(-1.88300011777082,0.661933049948511,92.1861195258989));
#9289=CARTESIAN_POINT('Ctrl Pts',(-1.90492252194614,0.595924117470595,92.1905389914565));
#9290=CARTESIAN_POINT('Ctrl Pts',(-1.92334651255382,0.528928875319798,92.194958457014));
#9291=CARTESIAN_POINT('Ctrl Pts',(-1.9417636630176,0.461958506015848,92.199376281788));
#9292=CARTESIAN_POINT('Ctrl Pts',(-1.95668485112832,0.394003031190437,92.203794106562));
#9293=CARTESIAN_POINT('Ctrl Pts',(-1.96801992106826,0.325461445917162,92.208211931336));
#9294=CARTESIAN_POINT('Ctrl Pts',(-1.97935880191346,0.256896816631853,92.2126312414041));
#9295=CARTESIAN_POINT('Ctrl Pts',(-1.98710907499091,0.18774617111172,92.2170505514721));
#9296=CARTESIAN_POINT('Ctrl Pts',(-1.99123202715443,0.11841696050171,92.2214698615402));
#9297=CARTESIAN_POINT('Ctrl Pts',(-1.993610686127,0.0784187887213646,92.2240194985791));
#9298=CARTESIAN_POINT('Ctrl Pts',(-1.99478295639525,0.0383612921081724,
92.226569135618));
#9299=CARTESIAN_POINT('Ctrl Pts',(-1.99474929503159,-0.00167704232401422,
92.229118772657));
#9300=CARTESIAN_POINT('',(-1.99474967489821,0.00113885621706795,92.0696038375131));
#9301=CARTESIAN_POINT('Ctrl Pts',(-1.66701737487202,1.09548191878041,91.9972724317));
#9302=CARTESIAN_POINT('Ctrl Pts',(-1.69219537653955,1.0571680356165,92.000471981164));
#9303=CARTESIAN_POINT('Ctrl Pts',(-1.71605789380988,1.017977927257,92.0036711945253));
#9304=CARTESIAN_POINT('Ctrl Pts',(-1.7674044424413,0.926698891525834,92.0109141311246));
#9305=CARTESIAN_POINT('Ctrl Pts',(-1.79397031634323,0.874163037773306,92.0149358977278));
#9306=CARTESIAN_POINT('Ctrl Pts',(-1.82632555717588,0.802468062534797,92.0201647506246));
#9307=CARTESIAN_POINT('Ctrl Pts',(-1.83420553094384,0.784289599424951,92.0214689004776));
#9308=CARTESIAN_POINT('Ctrl Pts',(-1.84698924707399,0.753551545934536,92.0236343527134));
#9309=CARTESIAN_POINT('Ctrl Pts',(-1.85203870088538,0.741054589587858,92.0245037834866));
#9310=CARTESIAN_POINT('Ctrl Pts',(-1.8627016202186,0.713874826225009,92.0263701732936));
#9311=CARTESIAN_POINT('Ctrl Pts',(-1.86826883068011,0.699175377519772,92.0273645315911));
#9312=CARTESIAN_POINT('Ctrl Pts',(-1.8845335188224,0.654648736378609,92.0303358761883));
#9313=CARTESIAN_POINT('Ctrl Pts',(-1.89469511400359,0.6246296737299,92.0322845171412));
#9314=CARTESIAN_POINT('Ctrl Pts',(-1.91768981397806,0.550964476823735,92.0369635411917));
#9315=CARTESIAN_POINT('Ctrl Pts',(-1.92975387028652,0.507096192033644,92.0396637559236));
#9316=CARTESIAN_POINT('Ctrl Pts',(-1.97639160174966,0.311587330246312,92.0514701542936));
#9317=CARTESIAN_POINT('Ctrl Pts',(-1.99466089793704,0.156635056505689,92.0602755466886));
#9318=CARTESIAN_POINT('Ctrl Pts',(-1.99474967489821,0.00113885621706795,
92.0696038375131));
#9319=CARTESIAN_POINT('Ctrl Pts',(-1.99474967628819,0.00113641901575271,
92.069603983722));
#9320=CARTESIAN_POINT('Ctrl Pts',(-1.99476815930295,-0.0313067090923167,
92.0715502633252));
#9321=CARTESIAN_POINT('Ctrl Pts',(-1.99399514718505,-0.0637444795486412,
92.0735154383802));
#9322=CARTESIAN_POINT('Ctrl Pts',(-1.99109370651439,-0.123869624873462,
92.0772043722034));
#9323=CARTESIAN_POINT('Ctrl Pts',(-1.98917761274169,-0.151559029694067,
92.0789215260781));
#9324=CARTESIAN_POINT('Ctrl Pts',(-1.9846989271426,-0.201212005455588,92.0820386507972));
#9325=CARTESIAN_POINT('Ctrl Pts',(-1.98234763062877,-0.223190300630611,
92.0834318024355));
#9326=CARTESIAN_POINT('Ctrl Pts',(-1.97694509971369,-0.266821314003556,
92.0862262487283));
#9327=CARTESIAN_POINT('Ctrl Pts',(-1.97390207845581,-0.288471943710301,
92.0876270977286));
#9328=CARTESIAN_POINT('Ctrl Pts',(-1.96486297577387,-0.345916170498519,
92.0913835897934));
#9329=CARTESIAN_POINT('Ctrl Pts',(-1.95824514205408,-0.381602132725231,
92.093758594248));
#9330=CARTESIAN_POINT('Ctrl Pts',(-1.92253348233093,-0.548621053328147,
92.105076283791));
#9331=CARTESIAN_POINT('Ctrl Pts',(-1.8811808201895,-0.676955081330919,92.1143990859579));
#9332=CARTESIAN_POINT('Ctrl Pts',(-1.79851367188029,-0.865740088117418,
92.12878224574));
#9333=CARTESIAN_POINT('Ctrl Pts',(-1.7662707031514,-0.929755870915924,92.1337808611449));
#9334=CARTESIAN_POINT('Ctrl Pts',(-1.71594042541975,-1.01757135162152,92.1407053723335));
#9335=CARTESIAN_POINT('Ctrl Pts',(-1.70065764708605,-1.04291262395225,92.1427116766899));
#9336=CARTESIAN_POINT('Ctrl Pts',(-1.67232555717517,-1.08761166310955,92.146253346622));
#9337=CARTESIAN_POINT('Ctrl Pts',(-1.6594896710628,-1.1070980284683,92.1477982892483));
#9338=CARTESIAN_POINT('Ctrl Pts',(-1.63835559680957,-1.13798820544017,92.1502433588491));
#9339=CARTESIAN_POINT('Ctrl Pts',(-1.63027356029034,-1.14953659072281,92.1511565267063));
#9340=CARTESIAN_POINT('Ctrl Pts',(-1.61363733911933,-1.17277959791909,92.1529909428631));
#9341=CARTESIAN_POINT('Ctrl Pts',(-1.60507686729099,-1.18446854280788,92.1539117224658));
#9342=CARTESIAN_POINT('Ctrl Pts',(-1.58123720889065,-1.21628740220106,92.1564165141851));
#9343=CARTESIAN_POINT('Ctrl Pts',(-1.565701167694,-1.23622253140346,92.1579839279255));
#9344=CARTESIAN_POINT('Ctrl Pts',(-1.46850819467474,-1.35616336391058,92.1674397269088));
#9345=CARTESIAN_POINT('Ctrl Pts',(-1.37767138002826,-1.44835238372914,92.174832417256));
#9346=CARTESIAN_POINT('Ctrl Pts',(-1.20651129000893,-1.59127831962814,92.1877771006588));
#9347=CARTESIAN_POINT('Ctrl Pts',(-1.13031988870464,-1.64627184677635,92.1932612864709));
#9348=CARTESIAN_POINT('Ctrl Pts',(-1.01577335023588,-1.71723769631638,92.2014027876154));
#9349=CARTESIAN_POINT('Ctrl Pts',(-0.98034823541893,-1.73770474739748,92.2039064470741));
#9350=CARTESIAN_POINT('Ctrl Pts',(-0.922187429267494,-1.76896277328122,
92.2080109138262));
#9351=CARTESIAN_POINT('Ctrl Pts',(-0.89983214263199,-1.7804384209886,92.2095870928512));
#9352=CARTESIAN_POINT('Ctrl Pts',(-0.85605686821332,-1.80187456212417,92.2126739799368));
#9353=CARTESIAN_POINT('Ctrl Pts',(-0.834664915709949,-1.81188291516373,
92.214182678758));
#9354=CARTESIAN_POINT('Ctrl Pts',(-0.782332780157432,-1.83524339258574,
92.2178763408885));
#9355=CARTESIAN_POINT('Ctrl Pts',(-0.751223123118983,-1.84819546526699,
92.2200745519905));
#9356=CARTESIAN_POINT('Ctrl Pts',(-0.572070556305459,-1.91751261430636,
92.2327549983201));
#9357=CARTESIAN_POINT('Ctrl Pts',(-0.418078800007309,-1.9568628735305,92.2438024117842));
#9358=CARTESIAN_POINT('Ctrl Pts',(-0.180610869034097,-1.98821459869155,
92.2605007860614));
#9359=CARTESIAN_POINT('Ctrl Pts',(-0.0995498011176361,-1.99391815172663,
92.2661293205249));
#9360=CARTESIAN_POINT('Ctrl Pts',(0.00600012830176016,-1.99488973904457,
92.2732053170416));
#9361=CARTESIAN_POINT('Ctrl Pts',(0.0303645644341954,-1.99466769008684,
92.2748209310496));
#9362=CARTESIAN_POINT('Ctrl Pts',(0.0690181916411301,-1.99360694258104,
92.2773496155312));
#9363=CARTESIAN_POINT('Ctrl Pts',(0.083312203281262,-1.9930607767081,92.2782772284045));
#9364=CARTESIAN_POINT('Ctrl Pts',(0.110098035469349,-1.99174862121941,92.2799999046068));
#9365=CARTESIAN_POINT('Ctrl Pts',(0.122590798061702,-1.99101875016146,92.2807969743612));
#9366=CARTESIAN_POINT('Ctrl Pts',(0.157239976173884,-1.98866705251675,92.2829920247745));
#9367=CARTESIAN_POINT('Ctrl Pts',(0.179378124642974,-1.98679255132669,92.2843767087599));
#9368=CARTESIAN_POINT('Ctrl Pts',(0.332357579302097,-1.97126130246421,92.2938504944873));
#9369=CARTESIAN_POINT('Ctrl Pts',(0.461615382922778,-1.94505853645239,92.3013900749511));
#9370=CARTESIAN_POINT('Ctrl Pts',(0.687630253288546,-1.87541993108513,92.3151134721051));
#9371=CARTESIAN_POINT('Ctrl Pts',(0.785293372111633,-1.83666726471702,92.3212396356086));
#9372=CARTESIAN_POINT('Ctrl Pts',(0.912623034940053,-1.77412305952781,92.3298548294559));
#9373=CARTESIAN_POINT('Ctrl Pts',(0.945333952688054,-1.7569111772095,92.3321265918226));
#9374=CARTESIAN_POINT('Ctrl Pts',(0.998820004138919,-1.72684155814258,92.3359515751138));
#9375=CARTESIAN_POINT('Ctrl Pts',(1.01987150916701,-1.71449269095366,92.3374864431387));
#9376=CARTESIAN_POINT('Ctrl Pts',(1.06152088476724,-1.68902254371992,92.340585479545));
#9377=CARTESIAN_POINT('Ctrl Pts',(1.08211487578369,-1.67590305494017,92.3421493946391));
#9378=CARTESIAN_POINT('Ctrl Pts',(1.1333173489969,-1.6419470449696,92.3461205773597));
#9379=CARTESIAN_POINT('Ctrl Pts',(1.16359504893925,-1.62063091736894,92.3485456144877));
#9380=CARTESIAN_POINT('Ctrl Pts',(1.29657722448443,-1.52136048375288,92.3595533379029));
#9381=CARTESIAN_POINT('Ctrl Pts',(1.39215854268234,-1.43441119369384,92.3684781384058));
#9382=CARTESIAN_POINT('Ctrl Pts',(1.52859241424551,-1.28373081793755,92.3826631260226));
#9383=CARTESIAN_POINT('Ctrl Pts',(1.57539338828112,-1.22584505927741,92.3878590973772));
#9384=CARTESIAN_POINT('Ctrl Pts',(1.63649785459933,-1.14097076994958,92.3950192067337));
#9385=CARTESIAN_POINT('Ctrl Pts',(1.65358425681368,-1.11606398332346,92.3970684686953));
#9386=CARTESIAN_POINT('Ctrl Pts',(1.68305038840129,-1.07094812764809,92.4006767969649));
#9387=CARTESIAN_POINT('Ctrl Pts',(1.69564797344349,-1.05088846742278,92.4022459356625));
#9388=CARTESIAN_POINT('Ctrl Pts',(1.71520477076662,-1.01847966244255,92.4047196196261));
#9389=CARTESIAN_POINT('Ctrl Pts',(1.72239452261107,-1.00627301064675,92.4056377148263));
#9390=CARTESIAN_POINT('Ctrl Pts',(1.73573820717803,-0.983056196120208,92.4073568373933));
#9391=CARTESIAN_POINT('Ctrl Pts',(1.74191885440136,-0.972062412678964,92.4081596425926));
#9392=CARTESIAN_POINT('Ctrl Pts',(1.75896963249874,-0.94104851785814,92.410395122327));
#9393=CARTESIAN_POINT('Ctrl Pts',(1.76960205299495,-0.920899103926255,92.4118136511195));
#9394=CARTESIAN_POINT('Ctrl Pts',(1.83699204524145,-0.787709596826022,92.4209997007485));
#9395=CARTESIAN_POINT('Ctrl Pts',(1.88323969305942,-0.669658356904713,92.4282659318206));
#9396=CARTESIAN_POINT('Ctrl Pts',(1.9476831258567,-0.44411064011118,92.4418721483562));
#9397=CARTESIAN_POINT('Ctrl Pts',(1.96887517062733,-0.337981237456235,92.448170376723));
#9398=CARTESIAN_POINT('Ctrl Pts',(1.98568838712542,-0.193557930276693,92.4569955553312));
#9399=CARTESIAN_POINT('Ctrl Pts',(1.98896466913657,-0.15634037400082,92.4592907518267));
#9400=CARTESIAN_POINT('Ctrl Pts',(1.99265484680723,-0.0946219287196938,
92.4631438043902));
#9401=CARTESIAN_POINT('Ctrl Pts',(1.99366581253361,-0.0701654480856943,
92.4646827019488));
#9402=CARTESIAN_POINT('Ctrl Pts',(1.99478425822608,-0.0213566764327326,
92.467781019639));
#9403=CARTESIAN_POINT('Ctrl Pts',(1.994896315478,0.00299127359219256,92.4693400233891));
#9404=CARTESIAN_POINT('Ctrl Pts',(1.9940607197209,0.0639640262856332,92.4732802494589));
#9405=CARTESIAN_POINT('Ctrl Pts',(1.99254981671886,0.100570790967986,92.4756786593363));
#9406=CARTESIAN_POINT('Ctrl Pts',(1.98351299647704,0.231729203991478,92.4843946324364));
#9407=CARTESIAN_POINT('Ctrl Pts',(1.97025543103971,0.325747885601911,92.4908797553944));
#9408=CARTESIAN_POINT('Ctrl Pts',(1.93321044483757,0.498409033692966,92.5031387257009));
#9409=CARTESIAN_POINT('Ctrl Pts',(1.91115664424411,0.577229874277698,92.5088742771932));
#9410=CARTESIAN_POINT('Ctrl Pts',(1.86965981403512,0.696705358554105,92.517641911271));
#9411=CARTESIAN_POINT('Ctrl Pts',(1.85357548667641,0.738433834987035,92.5207177122762));
#9412=CARTESIAN_POINT('Ctrl Pts',(1.82386280549038,0.808413695952085,92.5258631834048));
#9413=CARTESIAN_POINT('Ctrl Pts',(1.81094608765506,0.836948478242977,92.5279574710078));
#9414=CARTESIAN_POINT('Ctrl Pts',(1.79057389348865,0.87927108546852,92.5310456031421));
#9415=CARTESIAN_POINT('Ctrl Pts',(1.78361978028004,0.893293360548532,92.5320657014294));
#9416=CARTESIAN_POINT('Ctrl Pts',(1.77036206543856,0.919253998929284,92.5339465634377));
#9417=CARTESIAN_POINT('Ctrl Pts',(1.7641015614015,0.931211816650328,92.5348095751338));
#9418=CARTESIAN_POINT('Ctrl Pts',(1.74828863966369,0.960683242878534,92.5369298949156));
#9419=CARTESIAN_POINT('Ctrl Pts',(1.73859407198787,0.978118697683891,92.5381785490521));
#9420=CARTESIAN_POINT('Ctrl Pts',(1.6973480044638,1.04974728484298,92.5432967129143));
#9421=CARTESIAN_POINT('Ctrl Pts',(1.6635088644478,1.10258756480942,92.5470450258289));
#9422=CARTESIAN_POINT('Ctrl Pts',(1.5544104174522,1.25645852162732,92.5581458891424));
#9423=CARTESIAN_POINT('Ctrl Pts',(1.47202697515336,1.35204205087646,92.5653154421523));
#9424=CARTESIAN_POINT('Ctrl Pts',(1.34648623473052,1.47251987115408,92.5755693772603));
#9425=CARTESIAN_POINT('Ctrl Pts',(1.31060017425249,1.50454866920715,92.5784337306157));
#9426=CARTESIAN_POINT('Ctrl Pts',(1.24347023939924,1.56023754823306,92.5837153266097));
#9427=CARTESIAN_POINT('Ctrl Pts',(1.21261967764178,1.58433350265185,92.5861153275308));
#9428=CARTESIAN_POINT('Ctrl Pts',(1.16109548349719,1.62218985668829,92.5900944879414));
#9429=CARTESIAN_POINT('Ctrl Pts',(1.14083777701438,1.63649984131077,92.5916519042782));
#9430=CARTESIAN_POINT('Ctrl Pts',(1.10062225286171,1.66379835284803,92.5947331400346));
#9431=CARTESIAN_POINT('Ctrl Pts',(1.0806882295598,1.676814590656,92.5962555504483));
#9432=CARTESIAN_POINT('Ctrl Pts',(1.03098094237594,1.70801721083492,92.6000422852632));
#9433=CARTESIAN_POINT('Ctrl Pts',(1.00095538791277,1.72578461932781,92.6023215319823));
#9434=CARTESIAN_POINT('Ctrl Pts',(0.839566503058463,1.81565660722181,92.6145375633317));
#9435=CARTESIAN_POINT('Ctrl Pts',(0.700873915672799,1.87356401295225,92.6249672194005));
#9436=CARTESIAN_POINT('Ctrl Pts',(0.49610438072653,1.93311532000006,92.6398431270132));
#9437=CARTESIAN_POINT('Ctrl Pts',(0.434357593804084,1.94791905622915,92.6442570940759));
#9438=CARTESIAN_POINT('Ctrl Pts',(0.333336152459379,1.9670953042262,92.6512739442206));
#9439=CARTESIAN_POINT('Ctrl Pts',(0.294452992895344,1.97329035287538,92.6539262460606));
#9440=CARTESIAN_POINT('Ctrl Pts',(0.238560656324332,1.98050624430187,92.6576468419131));
#9441=CARTESIAN_POINT('Ctrl Pts',(0.221684207796456,1.98246622439639,92.6587583271979));
#9442=CARTESIAN_POINT('Ctrl Pts',(0.191560436821653,1.98557520357651,92.6607186031166));
#9443=CARTESIAN_POINT('Ctrl Pts',(0.178323941693687,1.98680771154917,92.6615716197845));
#9444=CARTESIAN_POINT('Ctrl Pts',(0.14756488091511,1.98936192843031,92.6635350663576));
#9445=CARTESIAN_POINT('Ctrl Pts',(0.130035708517556,1.99058459823705,92.6646401775549));
#9446=CARTESIAN_POINT('Ctrl Pts',(0.0723021803309049,1.99384561271655,92.6682411991543));
#9447=CARTESIAN_POINT('Ctrl Pts',(0.0320499559405096,1.99489879431462,92.6706901911525));
#9448=CARTESIAN_POINT('Ctrl Pts',(-0.155797303403388,1.99412570932591,92.6819446811642));
#9449=CARTESIAN_POINT('Ctrl Pts',(-0.302869596073771,1.97714092263479,92.6902856592983));
#9450=CARTESIAN_POINT('Ctrl Pts',(-0.496328578656435,1.93268606047646,92.7019533132019));
#9451=CARTESIAN_POINT('Ctrl Pts',(-0.54547001421628,1.91939559110178,92.7049762794578));
#9452=CARTESIAN_POINT('Ctrl Pts',(-0.632941426173635,1.89210799916847,92.7105136017045));
#9453=CARTESIAN_POINT('Ctrl Pts',(-0.671452364808724,1.87878655045879,92.7130077213859));
#9454=CARTESIAN_POINT('Ctrl Pts',(-0.732982038367703,1.85536916631048,92.7171006113603));
#9455=CARTESIAN_POINT('Ctrl Pts',(-0.756266077986385,1.8460007961403,92.7186750234803));
#9456=CARTESIAN_POINT('Ctrl Pts',(-0.801119128896851,1.82696309018992,92.7217611632136));
#9457=CARTESIAN_POINT('Ctrl Pts',(-0.822705296035073,1.81734474105831,92.7232709344411));
#9458=CARTESIAN_POINT('Ctrl Pts',(-0.874732667651834,1.79304552892249,92.7269722129532));
#9459=CARTESIAN_POINT('Ctrl Pts',(-0.904980578709403,1.77797059267601,92.729177105323));
#9460=CARTESIAN_POINT('Ctrl Pts',(-1.0741618171987,1.68821834140363,92.7418211758236));
#9461=CARTESIAN_POINT('Ctrl Pts',(-1.2042141765976,1.59804757812337,92.7528195916793));
#9462=CARTESIAN_POINT('Ctrl Pts',(-1.38333298708292,1.43946836765162,92.7694982137849));
#9463=CARTESIAN_POINT('Ctrl Pts',(-1.44103041200812,1.38170651202603,92.7751541092078));
#9464=CARTESIAN_POINT('Ctrl Pts',(-1.51119050239875,1.30227743026863,92.7822590581783));
#9465=CARTESIAN_POINT('Ctrl Pts',(-1.52701197316126,1.2836891378177,92.7838777248946));
#9466=CARTESIAN_POINT('Ctrl Pts',(-1.55156404018349,1.25374695583476,92.786409995634));
#9467=CARTESIAN_POINT('Ctrl Pts',(-1.56051993562089,1.2425819736411,92.7873382094275));
#9468=CARTESIAN_POINT('Ctrl Pts',(-1.57815319761975,1.22010785991952,92.7891732460102));
#9469=CARTESIAN_POINT('Ctrl Pts',(-1.58683105974168,1.20880019916237,92.7900800745711));
#9470=CARTESIAN_POINT('Ctrl Pts',(-1.60986288414226,1.17811314671413,92.7925000623752));
#9471=CARTESIAN_POINT('Ctrl Pts',(-1.62398831827379,1.15856426500583,92.7939984641872));
#9472=CARTESIAN_POINT('Ctrl Pts',(-1.64770140204872,1.12446036815093,92.7965481036753));
#9473=CARTESIAN_POINT('Ctrl Pts',(-1.65745570970042,1.11003209729936,92.7976075187219));
#9474=CARTESIAN_POINT('Ctrl Pts',(-1.66701723320527,1.09548213435758,92.7986587716037));
#9475=CARTESIAN_POINT('Origin',(0.,0.,89.2710285354474));
#9476=CARTESIAN_POINT('',(-1.66701713450993,1.09548228454426,93.7559248887299));
#9477=CARTESIAN_POINT('',(-1.66701733785599,1.09548197510845,93.5957235785224));
#9478=CARTESIAN_POINT('',(-1.66701720851066,1.09548217193587,89.2710285354474));
#9479=CARTESIAN_POINT('Ctrl Pts',(-1.66701713450993,1.09548228454426,93.7559248887299));
#9480=CARTESIAN_POINT('Ctrl Pts',(-1.63542234952196,1.14356069592451,93.7525427819055));
#9481=CARTESIAN_POINT('Ctrl Pts',(-1.60175109836394,1.19026704693653,93.7491185570963));
#9482=CARTESIAN_POINT('Ctrl Pts',(-1.54306510953131,1.26465803650423,93.7433659959786));
#9483=CARTESIAN_POINT('Ctrl Pts',(-1.51922723760391,1.29319689533183,93.7410811748776));
#9484=CARTESIAN_POINT('Ctrl Pts',(-1.47841484587907,1.33937108039223,93.7372402368012));
#9485=CARTESIAN_POINT('Ctrl Pts',(-1.4618878920162,1.35739053083534,93.7357028037696));
#9486=CARTESIAN_POINT('Ctrl Pts',(-1.42822317223878,1.39276733554216,93.732603267755));
#9487=CARTESIAN_POINT('Ctrl Pts',(-1.41108995532366,1.41012316162491,93.7310415046378));
#9488=CARTESIAN_POINT('Ctrl Pts',(-1.36729464985399,1.45288994709965,93.7270855334408));
#9489=CARTESIAN_POINT('Ctrl Pts',(-1.34023989165373,1.47788382209803,93.7246738541496));
#9490=CARTESIAN_POINT('Ctrl Pts',(-1.21310414035976,1.58897197145637,93.713477938339));
#9491=CARTESIAN_POINT('Ctrl Pts',(-1.10533562312598,1.66573610214229,93.7043317525641));
#9492=CARTESIAN_POINT('Ctrl Pts',(-0.900776132060031,1.78280329532145,93.6878833589033));
#9493=CARTESIAN_POINT('Ctrl Pts',(-0.806867613665749,1.8272256071364,93.6806395734607));
#9494=CARTESIAN_POINT('Ctrl Pts',(-0.688664218951933,1.87224107944017,93.6721834399008));
#9495=CARTESIAN_POINT('Ctrl Pts',(-0.667266915805027,1.87997341354761,93.6706783953537));
#9496=CARTESIAN_POINT('Ctrl Pts',(-0.632510311839856,1.89186516681706,93.66828012238));
#9497=CARTESIAN_POINT('Ctrl Pts',(-0.619231775508093,1.89625292433228,93.6673746904563));
#9498=CARTESIAN_POINT('Ctrl Pts',(-0.591956855281497,1.90494856766909,93.6655384661907));
#9499=CARTESIAN_POINT('Ctrl Pts',(-0.577957162684838,1.90924265463408,93.6646084317539));
#9500=CARTESIAN_POINT('Ctrl Pts',(-0.538942904382735,1.9207409141232,93.6620478302636));
#9501=CARTESIAN_POINT('Ctrl Pts',(-0.51383184360503,1.92761046360899,93.6604351136759));
#9502=CARTESIAN_POINT('Ctrl Pts',(-0.364238945804778,1.96540281758391,93.6509970658309));
#9503=CARTESIAN_POINT('Ctrl Pts',(-0.237131541205012,1.98475546695384,93.6436530643455));
#9504=CARTESIAN_POINT('Ctrl Pts',(-0.0159020677013387,1.99686611905797,
93.6307903400082));
#9505=CARTESIAN_POINT('Ctrl Pts',(0.0774671278218953,1.99542574557168,93.6253391504231));
#9506=CARTESIAN_POINT('Ctrl Pts',(0.211189295057473,1.9839616263326,93.6172304543193));
#9507=CARTESIAN_POINT('Ctrl Pts',(0.251872146285257,1.97920810452988,93.6147240332468));
#9508=CARTESIAN_POINT('Ctrl Pts',(0.317246763879554,1.96952128542069,93.6106159510326));
#9509=CARTESIAN_POINT('Ctrl Pts',(0.342042807810405,1.96536669054304,93.609038992585));
#9510=CARTESIAN_POINT('Ctrl Pts',(0.389969561788923,1.95640210028981,93.6059511533259));
#9511=CARTESIAN_POINT('Ctrl Pts',(0.413106449407846,1.95164761652855,93.6044422942812));
#9512=CARTESIAN_POINT('Ctrl Pts',(0.463821976024148,1.94028368203812,93.6010926142209));
#9513=CARTESIAN_POINT('Ctrl Pts',(0.491354682476796,1.93349477127464,93.5992462864226));
#9514=CARTESIAN_POINT('Ctrl Pts',(0.594922068193883,1.90560258747591,93.5921919718257));
#9515=CARTESIAN_POINT('Ctrl Pts',(0.669818411294887,1.88058346954879,93.5868620405255));
#9516=CARTESIAN_POINT('Ctrl Pts',(0.884090929361408,1.79457930315383,93.5709818855701));
#9517=CARTESIAN_POINT('Ctrl Pts',(1.0182113577112,1.72202650218283,93.5601865710314));
#9518=CARTESIAN_POINT('Ctrl Pts',(1.16969257161417,1.61614487213413,93.5476564622014));
#9519=CARTESIAN_POINT('Ctrl Pts',(1.19612934275542,1.5966777504839,93.5454579227881));
#9520=CARTESIAN_POINT('Ctrl Pts',(1.23466016862367,1.56681057405204,93.5422498259342));
#9521=CARTESIAN_POINT('Ctrl Pts',(1.24712834807564,1.55690463132253,93.5412111191029));
#9522=CARTESIAN_POINT('Ctrl Pts',(1.26989398043794,1.53836838629555,93.5393155168166));
#9523=CARTESIAN_POINT('Ctrl Pts',(1.28022437495878,1.52978219818604,93.5384559624389));
#9524=CARTESIAN_POINT('Ctrl Pts',(1.30529226701484,1.50851502628617,93.5363702730614));
#9525=CARTESIAN_POINT('Ctrl Pts',(1.31993242984823,1.4957218778217,93.5351520793587));
#9526=CARTESIAN_POINT('Ctrl Pts',(1.37590909033274,1.44534517420562,93.5304831569122));
#9527=CARTESIAN_POINT('Ctrl Pts',(1.41584981420338,1.4062428295479,93.52712738481));
#9528=CARTESIAN_POINT('Ctrl Pts',(1.5444669328074,1.26928169552506,93.5160208047763));
#9529=CARTESIAN_POINT('Ctrl Pts',(1.62506047987489,1.16431736586136,93.5085201825453));
#9530=CARTESIAN_POINT('Ctrl Pts',(1.72052360439719,1.01055619696129,93.4978634622076));
#9531=CARTESIAN_POINT('Ctrl Pts',(1.7448097841133,0.96802048697242,93.4949493176046));
#9532=CARTESIAN_POINT('Ctrl Pts',(1.78588409374039,0.889504135852703,93.4895870781914));
#9533=CARTESIAN_POINT('Ctrl Pts',(1.80321019461239,0.85383386781165,93.4871571365949));
#9534=CARTESIAN_POINT('Ctrl Pts',(1.82966779540116,0.794961202009411,93.4831415325032));
#9535=CARTESIAN_POINT('Ctrl Pts',(1.83944793001755,0.772061381717299,93.4815784277842));
#9536=CARTESIAN_POINT('Ctrl Pts',(1.85771576220401,0.726969035081655,93.478495111394));
#9537=CARTESIAN_POINT('Ctrl Pts',(1.86624068370553,0.704796041886973,93.4769764838878));
#9538=CARTESIAN_POINT('Ctrl Pts',(1.88618329361931,0.650025282652543,93.4732167961798));
#9539=CARTESIAN_POINT('Ctrl Pts',(1.89715384104378,0.617274121355461,93.4709613146153));
#9540=CARTESIAN_POINT('Ctrl Pts',(1.95192163866515,0.438488075045035,93.4586022210182));
#9541=CARTESIAN_POINT('Ctrl Pts',(1.97970989498057,0.28810302838385,93.4479843390764));
#9542=CARTESIAN_POINT('Ctrl Pts',(1.99604001308518,0.0492366612757203,93.4312855684801));
#9543=CARTESIAN_POINT('Ctrl Pts',(1.9962884106473,-0.0378834358126214,93.4252433147478));
#9544=CARTESIAN_POINT('Ctrl Pts',(1.98938237459944,-0.148096772724516,93.4178523196876));
#9545=CARTESIAN_POINT('Ctrl Pts',(1.98750856810158,-0.17141964038473,93.4163030070519));
#9546=CARTESIAN_POINT('Ctrl Pts',(1.98384746537211,-0.208748418053945,93.4138525697228));
#9547=CARTESIAN_POINT('Ctrl Pts',(1.98232112604231,-0.22277714930768,93.4129383160795));
#9548=CARTESIAN_POINT('Ctrl Pts',(1.97892720571701,-0.251165926479747,93.4111033170167));
#9549=CARTESIAN_POINT('Ctrl Pts',(1.97705189507359,-0.265524092341655,93.4101830148195));
#9550=CARTESIAN_POINT('Ctrl Pts',(1.97148237757333,-0.304828984847685,93.4076819529907));
#9551=CARTESIAN_POINT('Ctrl Pts',(1.96747108398963,-0.329728897913695,93.4061177032218));
#9552=CARTESIAN_POINT('Ctrl Pts',(1.94536349641327,-0.452129863912211,93.3984984328528));
#9553=CARTESIAN_POINT('Ctrl Pts',(1.92048468622102,-0.548272938864789,93.3927297738895));
#9554=CARTESIAN_POINT('Ctrl Pts',(1.85867525994805,-0.730046628860321,93.3815915412368));
#9555=CARTESIAN_POINT('Ctrl Pts',(1.82270008116151,-0.815723743515311,93.3762326014404));
#9556=CARTESIAN_POINT('Ctrl Pts',(1.76199549100926,-0.936033779889465,93.3682377811264));
#9557=CARTESIAN_POINT('Ctrl Pts',(1.74192245224126,-0.972878820870892,93.3657220846679));
#9558=CARTESIAN_POINT('Ctrl Pts',(1.7027555322045,-1.03966823085816,93.3610100861994));
#9559=CARTESIAN_POINT('Ctrl Pts',(1.68399491551085,-1.06978844545612,93.358825257753));
#9560=CARTESIAN_POINT('Ctrl Pts',(1.65113115363754,-1.11954310308252,93.3551036202207));
#9561=CARTESIAN_POINT('Ctrl Pts',(1.63745598321047,-1.13945103735588,93.353582967134));
#9562=CARTESIAN_POINT('Ctrl Pts',(1.61074813931592,-1.17685759659768,93.3506622647059));
#9563=CARTESIAN_POINT('Ctrl Pts',(1.59778316899034,-1.1944003738574,93.3492649895696));
#9564=CARTESIAN_POINT('Ctrl Pts',(1.56270203298898,-1.24027478428027,93.3455354534106));
#9565=CARTESIAN_POINT('Ctrl Pts',(1.54010425564317,-1.26822623680201,93.3431843645177));
#9566=CARTESIAN_POINT('Ctrl Pts',(1.42494620494502,-1.40304744435642,93.3314409294363));
#9567=CARTESIAN_POINT('Ctrl Pts',(1.32197317531648,-1.50046278816646,93.3216212580264));
#9568=CARTESIAN_POINT('Ctrl Pts',(1.13400042410198,-1.64380890371644,93.3051250021431));
#9569=CARTESIAN_POINT('Ctrl Pts',(1.05437805064002,-1.69598190605259,93.2985041838583));
#9570=CARTESIAN_POINT('Ctrl Pts',(0.950923003430365,-1.75365875039872,93.2905769948661));
#9571=CARTESIAN_POINT('Ctrl Pts',(0.930314193468688,-1.76467821069174,93.2890296093495));
#9572=CARTESIAN_POINT('Ctrl Pts',(0.896962074551349,-1.78176472829155,93.2865814463969));
#9573=CARTESIAN_POINT('Ctrl Pts',(0.88434024567389,-1.78806288405536,93.2856675805637));
#9574=CARTESIAN_POINT('Ctrl Pts',(0.858622418064512,-1.80055684321425,93.2838325567028));
#9575=CARTESIAN_POINT('Ctrl Pts',(0.84552370977621,-1.8067448879044,93.2829118550947));
#9576=CARTESIAN_POINT('Ctrl Pts',(0.809411081498878,-1.8233263154625,93.2804083573384));
#9577=CARTESIAN_POINT('Ctrl Pts',(0.786264652228859,-1.83342662411646,93.2788421250531));
#9578=CARTESIAN_POINT('Ctrl Pts',(0.675134937370769,-1.87942794485256,93.271474877985));
#9579=CARTESIAN_POINT('Ctrl Pts',(0.584844393176332,-1.90945471522781,93.2659351030583));
#9580=CARTESIAN_POINT('Ctrl Pts',(0.366720947273009,-1.96505943854661,93.2528700881494));
#9581=CARTESIAN_POINT('Ctrl Pts',(0.237863649597003,-1.98478224007977,93.2453809313963));
#9582=CARTESIAN_POINT('Ctrl Pts',(0.0682470178642263,-1.99397981054131,
93.2351038178705));
#9583=CARTESIAN_POINT('Ctrl Pts',(0.0284327365951741,-1.99494470895301,
93.2326638763106));
#9584=CARTESIAN_POINT('Ctrl Pts',(-0.0363124433474292,-1.99457527449754,
93.2286361928083));
#9585=CARTESIAN_POINT('Ctrl Pts',(-0.0612372602153259,-1.99396565341182,
93.2270712849548));
#9586=CARTESIAN_POINT('Ctrl Pts',(-0.109856255472506,-1.991864082626,93.2239874877438));
#9587=CARTESIAN_POINT('Ctrl Pts',(-0.133548197247356,-1.99041596627606,
93.2224702412883));
#9588=CARTESIAN_POINT('Ctrl Pts',(-0.191517940135283,-1.98583306987759,
93.2187198485343));
#9589=CARTESIAN_POINT('Ctrl Pts',(-0.225750181422961,-1.98223326406348,
93.2164724484884));
#9590=CARTESIAN_POINT('Ctrl Pts',(-0.411879725121675,-1.95777639357405,
93.2040664700141));
#9591=CARTESIAN_POINT('Ctrl Pts',(-0.561056558839647,-1.92034719147979,
93.1933864311598));
#9592=CARTESIAN_POINT('Ctrl Pts',(-0.783055747182841,-1.83654870995879,
93.1768375736369));
#9593=CARTESIAN_POINT('Ctrl Pts',(-0.859718407371368,-1.80193618974015,
93.1710040094987));
#9594=CARTESIAN_POINT('Ctrl Pts',(-0.955795656056625,-1.75102600781155,
93.1637111095717));
#9595=CARTESIAN_POINT('Ctrl Pts',(-0.977401302949993,-1.73905843550621,
93.162072641649));
#9596=CARTESIAN_POINT('Ctrl Pts',(-1.01122214150283,-1.71949525666128,93.1595167903076));
#9597=CARTESIAN_POINT('Ctrl Pts',(-1.02358634144263,-1.71216389102741,93.158584366459));
#9598=CARTESIAN_POINT('Ctrl Pts',(-1.04800884303798,-1.69732341220236,93.1567481423143));
#9599=CARTESIAN_POINT('Ctrl Pts',(-1.06006828143407,-1.6898179089451,93.1558442256011));
#9600=CARTESIAN_POINT('Ctrl Pts',(-1.09216670589695,-1.66936175380594,93.1534428921319));
#9601=CARTESIAN_POINT('Ctrl Pts',(-1.11205589586242,-1.65617890984342,93.1519598293279));
#9602=CARTESIAN_POINT('Ctrl Pts',(-1.22654571179452,-1.57730067901706,93.1434217396586));
#9603=CARTESIAN_POINT('Ctrl Pts',(-1.31556089751201,-1.50386084621574,93.1367707306215));
#9604=CARTESIAN_POINT('Ctrl Pts',(-1.47757919337974,-1.34473346967987,93.1236042268181));
#9605=CARTESIAN_POINT('Ctrl Pts',(-1.55066524040848,-1.25975505137283,93.1171101707527));
#9606=CARTESIAN_POINT('Ctrl Pts',(-1.63973962949609,-1.13661308781823,93.107918319004));
#9607=CARTESIAN_POINT('Ctrl Pts',(-1.66225400167881,-1.10342496961415,93.1054620547317));
#9608=CARTESIAN_POINT('Ctrl Pts',(-1.69714745910588,-1.04849519934693,93.1014146453806));
#9609=CARTESIAN_POINT('Ctrl Pts',(-1.71014512693099,-1.02715881691861,93.0998467880661));
#9610=CARTESIAN_POINT('Ctrl Pts',(-1.73468822411039,-0.985112303192881,
93.0967621305723));
#9611=CARTESIAN_POINT('Ctrl Pts',(-1.74627190542321,-0.964429280296744,
93.0952470681473));
#9612=CARTESIAN_POINT('Ctrl Pts',(-1.77367434611226,-0.913388446268949,
93.0915114532353));
#9613=CARTESIAN_POINT('Ctrl Pts',(-1.78908504955663,-0.882821377165541,
93.0892769127863));
#9614=CARTESIAN_POINT('Ctrl Pts',(-1.86975554889749,-0.712015157965876,
93.0767972806393));
#9615=CARTESIAN_POINT('Ctrl Pts',(-1.91930871268802,-0.564968601757438,
93.0660192736889));
#9616=CARTESIAN_POINT('Ctrl Pts',(-1.96962984439087,-0.327614473729624,
93.0490995597353));
#9617=CARTESIAN_POINT('Ctrl Pts',(-1.98216658254263,-0.240398406497281,
93.0429930711034));
#9618=CARTESIAN_POINT('Ctrl Pts',(-1.99059247291952,-0.130603619848218,
93.0356398187603));
#9619=CARTESIAN_POINT('Ctrl Pts',(-1.99191700890647,-0.108546887912068,
93.0341796057686));
#9620=CARTESIAN_POINT('Ctrl Pts',(-1.99347565435247,-0.0726254471688885,
93.0318339437613));
#9621=CARTESIAN_POINT('Ctrl Pts',(-1.99393215967216,-0.0587726656381613,
93.0309372164655));
#9622=CARTESIAN_POINT('Ctrl Pts',(-1.99457817977182,-0.0300893687053928,
93.0290981675887));
#9623=CARTESIAN_POINT('Ctrl Pts',(-1.99474676737995,-0.0152595094716535,
93.0281569498896));
#9624=CARTESIAN_POINT('Ctrl Pts',(-1.99475574941179,0.0265445322984926,
93.0255273525876));
#9625=CARTESIAN_POINT('Ctrl Pts',(-1.99421444596626,0.0535165395315901,
93.0238584318743));
#9626=CARTESIAN_POINT('Ctrl Pts',(-1.99166871276284,0.116570099224328,93.0200045051092));
#9627=CARTESIAN_POINT('Ctrl Pts',(-1.98923067787367,0.152625152091631,93.0178372290286));
#9628=CARTESIAN_POINT('Ctrl Pts',(-1.97569999132832,0.295096090152994,93.0093496744791));
#9629=CARTESIAN_POINT('Ctrl Pts',(-1.95703410190557,0.400614195767204,93.0032246938392));
#9630=CARTESIAN_POINT('Ctrl Pts',(-1.90603995020134,0.59583853457678,92.9914713735557));
#9631=CARTESIAN_POINT('Ctrl Pts',(-1.8755814767033,0.685713634188596,92.9858815489744));
#9632=CARTESIAN_POINT('Ctrl Pts',(-1.8262909088681,0.802956805797081,92.9781042495431));
#9633=CARTESIAN_POINT('Ctrl Pts',(-1.81300356778381,0.832523869077009,92.9761002412399));
#9634=CARTESIAN_POINT('Ctrl Pts',(-1.78877841201611,0.883096504406376,92.9725901461986));
#9635=CARTESIAN_POINT('Ctrl Pts',(-1.77817579208428,0.90425572571023,92.9710959010078));
#9636=CARTESIAN_POINT('Ctrl Pts',(-1.75530454969179,0.947940497351477,92.9679544110535));
#9637=CARTESIAN_POINT('Ctrl Pts',(-1.74297295375286,0.97042796173567,92.9663051230171));
#9638=CARTESIAN_POINT('Ctrl Pts',(-1.71018699218662,1.02757345904019,92.9620278099911));
#9639=CARTESIAN_POINT('Ctrl Pts',(-1.68911241391379,1.06185945441587,92.959377899959));
#9640=CARTESIAN_POINT('Ctrl Pts',(-1.66701720827313,1.09548217229732,92.9566930507716));
#9641=CARTESIAN_POINT('Ctrl Pts',(-1.66701723320527,1.09548213435758,92.7986587716037));
#9642=CARTESIAN_POINT('Ctrl Pts',(-1.73358277777417,0.994188004171587,92.8059773982349));
#9643=CARTESIAN_POINT('Ctrl Pts',(-1.79080430631276,0.886996499275212,92.8129129536139));
#9644=CARTESIAN_POINT('Ctrl Pts',(-1.86506916841054,0.71092520135945,92.8240199321402));
#9645=CARTESIAN_POINT('Ctrl Pts',(-1.88879600493002,0.645249106260805,92.8281028737192));
#9646=CARTESIAN_POINT('Ctrl Pts',(-1.92366094116969,0.530189561905406,92.8352931399461));
#9647=CARTESIAN_POINT('Ctrl Pts',(-1.93645245705138,0.481376828343128,92.8383541327785));
#9648=CARTESIAN_POINT('Ctrl Pts',(-1.95319573152308,0.405924604148637,92.8431340104945));
#9649=CARTESIAN_POINT('Ctrl Pts',(-1.95848189088488,0.379601004188181,92.8448103274703));
#9650=CARTESIAN_POINT('Ctrl Pts',(-1.96737471167752,0.330168104992137,92.8479786594319));
#9651=CARTESIAN_POINT('Ctrl Pts',(-1.97110936606265,0.307086346196896,92.849466277822));
#9652=CARTESIAN_POINT('Ctrl Pts',(-1.97870700001022,0.25425551998164,92.8528923046844));
#9653=CARTESIAN_POINT('Ctrl Pts',(-1.98230626294191,0.224474893553132,92.8548387461944));
#9654=CARTESIAN_POINT('Ctrl Pts',(-1.99162693376925,0.129401653965325,92.8611047927957));
#9655=CARTESIAN_POINT('Ctrl Pts',(-1.9948024372975,0.0639086640660525,92.8655008761481));
#9656=CARTESIAN_POINT('Ctrl Pts',(-1.99465511719842,-0.117910358781764,
92.8779097976458));
#9657=CARTESIAN_POINT('Ctrl Pts',(-1.98439094668236,-0.233967639382531,
92.8860753729621));
#9658=CARTESIAN_POINT('Ctrl Pts',(-1.95114650175334,-0.421349275226169,
92.8993075156381));
#9659=CARTESIAN_POINT('Ctrl Pts',(-1.93416554738107,-0.49347093512938,92.904407391848));
#9660=CARTESIAN_POINT('Ctrl Pts',(-1.90735651027819,-0.584334586802061,
92.9107165915922));
#9661=CARTESIAN_POINT('Ctrl Pts',(-1.90119187458933,-0.604090477603018,
92.9120810164205));
#9662=CARTESIAN_POINT('Ctrl Pts',(-1.89050642106548,-0.636549028649673,
92.9143065213592));
#9663=CARTESIAN_POINT('Ctrl Pts',(-1.88616239214241,-0.64930783777143,92.9151770858983));
#9664=CARTESIAN_POINT('Ctrl Pts',(-1.87662478957617,-0.676416886776717,
92.9170165874034));
#9665=CARTESIAN_POINT('Ctrl Pts',(-1.87139533360319,-0.690753173554557,
92.9179834829762));
#9666=CARTESIAN_POINT('Ctrl Pts',(-1.85567909982095,-0.732349385696667,
92.920775534039));
#9667=CARTESIAN_POINT('Ctrl Pts',(-1.84475712448675,-0.759441834062847,
92.9225771968203));
#9668=CARTESIAN_POINT('Ctrl Pts',(-1.77954035833619,-0.911496147107613,
92.9326454919777));
#9669=CARTESIAN_POINT('Ctrl Pts',(-1.7131456271791,-1.03088743015271,92.9404025854022));
#9670=CARTESIAN_POINT('Ctrl Pts',(-1.57907898295936,-1.22274258367096,92.9540254115825));
#9671=CARTESIAN_POINT('Ctrl Pts',(-1.51725463547167,-1.298662873535,92.9597840613694));
#9672=CARTESIAN_POINT('Ctrl Pts',(-1.4278060820309,-1.39336035696389,92.9677486377447));
#9673=CARTESIAN_POINT('Ctrl Pts',(-1.40492200481048,-1.41643117198373,92.9697573357295));
#9674=CARTESIAN_POINT('Ctrl Pts',(-1.36440978718365,-1.45532602882664,92.9732724667747));
#9675=CARTESIAN_POINT('Ctrl Pts',(-1.34704405377998,-1.47141433876481,92.9747669439829));
#9676=CARTESIAN_POINT('Ctrl Pts',(-1.31030835442004,-1.50425233687816,92.9779058305046));
#9677=CARTESIAN_POINT('Ctrl Pts',(-1.29089402889713,-1.52094562068431,92.9795522255363));
#9678=CARTESIAN_POINT('Ctrl Pts',(-1.23765428873952,-1.56496970824304,92.9840368599456));
#9679=CARTESIAN_POINT('Ctrl Pts',(-1.20324931729963,-1.59157435313095,92.9869033836938));
#9680=CARTESIAN_POINT('Ctrl Pts',(-1.10404073383569,-1.66323408925702,92.9950861571707));
#9681=CARTESIAN_POINT('Ctrl Pts',(-1.03739809873881,-1.70559565083309,93.00049103467));
#9682=CARTESIAN_POINT('Ctrl Pts',(-0.843682912417196,-1.81317043202614,
93.0158621023904));
#9683=CARTESIAN_POINT('Ctrl Pts',(-0.711862417101707,-1.86886134718499,
93.0259635940504));
#9684=CARTESIAN_POINT('Ctrl Pts',(-0.552778315810356,-1.91677156248625,
93.0370843163391));
#9685=CARTESIAN_POINT('Ctrl Pts',(-0.53021353876527,-1.92313567073269,93.0386368570876));
#9686=CARTESIAN_POINT('Ctrl Pts',(-0.493888036648513,-1.93269280185331,
93.0410909391426));
#9687=CARTESIAN_POINT('Ctrl Pts',(-0.480197033226998,-1.93613989811209,
93.042005679616));
#9688=CARTESIAN_POINT('Ctrl Pts',(-0.45240942402555,-1.9428233091784,93.0438400739522));
#9689=CARTESIAN_POINT('Ctrl Pts',(-0.438312009033998,-1.94605223762001,
93.0447593108979));
#9690=CARTESIAN_POINT('Ctrl Pts',(-0.399612655355769,-1.95447421009414,
93.0472547239346));
#9691=CARTESIAN_POINT('Ctrl Pts',(-0.374944884625538,-1.95935606310019,
93.0488145089472));
#9692=CARTESIAN_POINT('Ctrl Pts',(-0.263505088602613,-1.97922860658991,
93.0557496110934));
#9693=CARTESIAN_POINT('Ctrl Pts',(-0.175882639845324,-1.98893166625432,
93.0609026963323));
#9694=CARTESIAN_POINT('Ctrl Pts',(0.0583901544985113,-1.99926488571686,
93.0745295959856));
#9695=CARTESIAN_POINT('Ctrl Pts',(0.204930305133938,-1.98959019038703,93.0829300454182));
#9696=CARTESIAN_POINT('Ctrl Pts',(0.383868432653864,-1.95778458687587,93.0939929498025));
#9697=CARTESIAN_POINT('Ctrl Pts',(0.418476757048317,-1.95067999160903,93.0961686434896));
#9698=CARTESIAN_POINT('Ctrl Pts',(0.47613270818206,-1.93723912907946,93.0998641340636));
#9699=CARTESIAN_POINT('Ctrl Pts',(0.499288670728882,-1.9314006685248,93.1013677328839));
#9700=CARTESIAN_POINT('Ctrl Pts',(0.546167865218077,-1.91868135019056,93.1044541587557));
#9701=CARTESIAN_POINT('Ctrl Pts',(0.569879179439027,-1.91177276114,93.1060376638746));
#9702=CARTESIAN_POINT('Ctrl Pts',(0.630276283468075,-1.89295187777978,93.1101314104183));
#9703=CARTESIAN_POINT('Ctrl Pts',(0.666754488391153,-1.88041301714173,93.1126617806849));
#9704=CARTESIAN_POINT('Ctrl Pts',(0.746929001184873,-1.85022797569027,93.1183560252242));
#9705=CARTESIAN_POINT('Ctrl Pts',(0.790408924064606,-1.83207523838219,93.1215344480049));
#9706=CARTESIAN_POINT('Ctrl Pts',(0.941881898457166,-1.76243960428723,93.1329189886566));
#9707=CARTESIAN_POINT('Ctrl Pts',(1.04584163009959,-1.70280546550533,93.1413272902403));
#9708=CARTESIAN_POINT('Ctrl Pts',(1.20108839945414,-1.59414551522322,93.154487457048));
#9709=CARTESIAN_POINT('Ctrl Pts',(1.25621242893426,-1.55107878721968,93.159293162197));
#9710=CARTESIAN_POINT('Ctrl Pts',(1.32444456969645,-1.49174224578306,93.1653129767044));
#9711=CARTESIAN_POINT('Ctrl Pts',(1.33971552051755,-1.47804287850864,93.1666650940437));
#9712=CARTESIAN_POINT('Ctrl Pts',(1.36464422671566,-1.45497579511731,93.1688764918592));
#9713=CARTESIAN_POINT('Ctrl Pts',(1.37442314417884,-1.44574184910487,93.1697450091712));
#9714=CARTESIAN_POINT('Ctrl Pts',(1.3951503083557,-1.42576937111761,93.1715870444625));
#9715=CARTESIAN_POINT('Ctrl Pts',(1.4060693497814,-1.41500236834655,93.1725583994572));
#9716=CARTESIAN_POINT('Ctrl Pts',(1.43769908609697,-1.3830853409288,93.1753790473706));
#9717=CARTESIAN_POINT('Ctrl Pts',(1.45806531681313,-1.36159812910831,93.1772041029978));
#9718=CARTESIAN_POINT('Ctrl Pts',(1.50562211867457,-1.30913242663865,93.1815106887642));
#9719=CARTESIAN_POINT('Ctrl Pts',(1.53234614423503,-1.2777485455341,93.1839680951894));
#9720=CARTESIAN_POINT('Ctrl Pts',(1.65186787372459,-1.12823766174791,93.1952561620992));
#9721=CARTESIAN_POINT('Ctrl Pts',(1.73210444863872,-1.00070173857716,93.2037554202385));
#9722=CARTESIAN_POINT('Ctrl Pts',(1.82127914161318,-0.815495775363631,93.2159951782602));
#9723=CARTESIAN_POINT('Ctrl Pts',(1.84320294362894,-0.764652333486747,93.219340771976));
#9724=CARTESIAN_POINT('Ctrl Pts',(1.87287077963935,-0.687130167819476,93.2244639515179));
#9725=CARTESIAN_POINT('Ctrl Pts',(1.88221933293004,-0.661092344034207,93.2261881381217));
#9726=CARTESIAN_POINT('Ctrl Pts',(1.89837164012252,-0.612981063845531,93.2293848103148));
#9727=CARTESIAN_POINT('Ctrl Pts',(1.90533935371217,-0.590967462871391,93.230851530997));
#9728=CARTESIAN_POINT('Ctrl Pts',(1.92012849492411,-0.541259688248745,93.2341748520179));
#9729=CARTESIAN_POINT('Ctrl Pts',(1.92773575762002,-0.513507732691427,93.2360381351656));
#9730=CARTESIAN_POINT('Ctrl Pts',(1.94999968326752,-0.424803623022148,93.2420223367544));
#9731=CARTESIAN_POINT('Ctrl Pts',(1.96238375849129,-0.363325595392939,93.2462135762827));
#9732=CARTESIAN_POINT('Ctrl Pts',(1.98711090575525,-0.201537723390736,93.2573481716866));
#9733=CARTESIAN_POINT('Ctrl Pts',(1.99476427900868,-0.100696007704139,93.2643982695156));
#9734=CARTESIAN_POINT('Ctrl Pts',(1.99473755778325,0.0880071858877521,93.2775631558897));
#9735=CARTESIAN_POINT('Ctrl Pts',(1.98893822119425,0.175642896268484,93.2836625484435));
#9736=CARTESIAN_POINT('Ctrl Pts',(1.97412291727871,0.287194964745106,93.291211463674));
#9737=CARTESIAN_POINT('Ctrl Pts',(1.97040074623101,0.311710240298752,93.2928566253757));
#9738=CARTESIAN_POINT('Ctrl Pts',(1.96379719620553,0.350335875008289,93.2954202251518));
#9739=CARTESIAN_POINT('Ctrl Pts',(1.96121859472815,0.364494592427848,93.2963538532427));
#9740=CARTESIAN_POINT('Ctrl Pts',(1.95579550137601,0.392546269099557,93.2981897951889));
#9741=CARTESIAN_POINT('Ctrl Pts',(1.95295566424722,0.406439189911222,93.2990922670959));
#9742=CARTESIAN_POINT('Ctrl Pts',(1.94496335750908,0.443519135267231,93.3014855898408));
#9743=CARTESIAN_POINT('Ctrl Pts',(1.93954433362855,0.466647168918481,93.302962250298));
#9744=CARTESIAN_POINT('Ctrl Pts',(1.92627135661989,0.519061893116134,93.3062833751774));
#9745=CARTESIAN_POINT('Ctrl Pts',(1.91816013344389,0.548277733178115,93.3081163180706));
#9746=CARTESIAN_POINT('Ctrl Pts',(1.88770524171498,0.649005716514939,93.314407754467));
#9747=CARTESIAN_POINT('Ctrl Pts',(1.86200128263339,0.719438665912472,93.3187589550081));
#9748=CARTESIAN_POINT('Ctrl Pts',(1.78179817005032,0.905878896388542,93.3305297870666));
#9749=CARTESIAN_POINT('Ctrl Pts',(1.72000033107232,1.01834003963853,93.3379279308839));
#9750=CARTESIAN_POINT('Ctrl Pts',(1.62696477649855,1.15472396604202,93.3479524974945));
#9751=CARTESIAN_POINT('Ctrl Pts',(1.60522567776207,1.18475823499143,93.3502309239898));
#9752=CARTESIAN_POINT('Ctrl Pts',(1.56779625578206,1.23354734594667,93.3540638853263));
#9753=CARTESIAN_POINT('Ctrl Pts',(1.55257493746703,1.2526512414243,93.3555998956789));
#9754=CARTESIAN_POINT('Ctrl Pts',(1.52145663340575,1.29026837036096,93.3586986964883));
#9755=CARTESIAN_POINT('Ctrl Pts',(1.50556311268616,1.30877896559753,93.3602611868543));
#9756=CARTESIAN_POINT('Ctrl Pts',(1.46478020192573,1.35455118446636,93.3642234014067));
#9757=CARTESIAN_POINT('Ctrl Pts',(1.43946702593971,1.38142112748593,93.366640725911));
#9758=CARTESIAN_POINT('Ctrl Pts',(1.33964565784226,1.48165753098581,93.3760227910914));
#9759=CARTESIAN_POINT('Ctrl Pts',(1.260166109322,1.54981792109557,93.3831981195032));
#9760=CARTESIAN_POINT('Ctrl Pts',(1.06896078215935,1.68932416319989,93.399667610501));
#9761=CARTESIAN_POINT('Ctrl Pts',(0.954716970738655,1.7564204682159,93.4089878084472));
#9762=CARTESIAN_POINT('Ctrl Pts',(0.814555674194009,1.82099344276447,93.4192938217076));
#9763=CARTESIAN_POINT('Ctrl Pts',(0.794286479735627,1.82992544989915,93.4207577010488));
#9764=CARTESIAN_POINT('Ctrl Pts',(0.762349176348671,1.84336854386684,93.4230184418628));
#9765=CARTESIAN_POINT('Ctrl Pts',(0.750780871540235,1.84811037550477,93.4238280564819));
#9766=CARTESIAN_POINT('Ctrl Pts',(0.725867578271714,1.85804975453646,93.4255506309008));
#9767=CARTESIAN_POINT('Ctrl Pts',(0.712509558042411,1.86321302904902,93.4264614650853));
#9768=CARTESIAN_POINT('Ctrl Pts',(0.676200921556376,1.87679980078664,93.4289057746728));
#9769=CARTESIAN_POINT('Ctrl Pts',(0.653148461228603,1.88494625719749,93.4304239720942));
#9770=CARTESIAN_POINT('Ctrl Pts',(0.552247099320134,1.91853002619811,93.4369474337038));
#9771=CARTESIAN_POINT('Ctrl Pts',(0.473016428015961,1.9395856219531,93.4417596454754));
#9772=CARTESIAN_POINT('Ctrl Pts',(0.238685200471375,1.98663956043353,93.4556722611848));
#9773=CARTESIAN_POINT('Ctrl Pts',(0.0815621009566453,1.99926265710679,93.4646488341483));
#9774=CARTESIAN_POINT('Ctrl Pts',(-0.109266383595662,1.99204322542493,93.4762986420151));
#9775=CARTESIAN_POINT('Ctrl Pts',(-0.143081436923691,1.9899002101402,93.4783891117578));
#9776=CARTESIAN_POINT('Ctrl Pts',(-0.200375541292755,1.98480131772284,93.4819843642072));
#9777=CARTESIAN_POINT('Ctrl Pts',(-0.223887039877736,1.98228684702796,93.4834750179601));
#9778=CARTESIAN_POINT('Ctrl Pts',(-0.272225280677243,1.97624632266604,93.4865739106634));
#9779=CARTESIAN_POINT('Ctrl Pts',(-0.297041241904327,1.97266888666929,93.4881835342224));
#9780=CARTESIAN_POINT('Ctrl Pts',(-0.361855275781671,1.96207468546193,93.4924393277618));
#9781=CARTESIAN_POINT('Ctrl Pts',(-0.401716301027536,1.95430292631391,93.4951088854404));
#9782=CARTESIAN_POINT('Ctrl Pts',(-0.549132303021071,1.92086053543104,93.5051820519882));
#9783=CARTESIAN_POINT('Ctrl Pts',(-0.654720647077651,1.88748152761864,93.5128132189124));
#9784=CARTESIAN_POINT('Ctrl Pts',(-0.863927386426982,1.80167066632472,93.5285798127436));
#9785=CARTESIAN_POINT('Ctrl Pts',(-0.966859360471028,1.74859211228761,93.5366918853279));
#9786=CARTESIAN_POINT('Ctrl Pts',(-1.08477530747532,1.6741738636361,93.5460311202479));
#9787=CARTESIAN_POINT('Ctrl Pts',(-1.10470192726965,1.66109282284214,93.5476104878353));
#9788=CARTESIAN_POINT('Ctrl Pts',(-1.13611597003732,1.63965532483181,93.5500962643702));
#9789=CARTESIAN_POINT('Ctrl Pts',(-1.14775635218576,1.63152826256372,93.5510164402055));
#9790=CARTESIAN_POINT('Ctrl Pts',(-1.17100542302791,1.61492427992367,93.5528507947463));
#9791=CARTESIAN_POINT('Ctrl Pts',(-1.1826111999242,1.60644480488654,93.5537647347169));
#9792=CARTESIAN_POINT('Ctrl Pts',(-1.21391256493022,1.58305214544875,93.5562279100334));
#9793=CARTESIAN_POINT('Ctrl Pts',(-1.23342503802517,1.56789687672873,93.5577614601002));
#9794=CARTESIAN_POINT('Ctrl Pts',(-1.3181141946708,1.49955930223707,93.5644338091069));
#9795=CARTESIAN_POINT('Ctrl Pts',(-1.38017637517835,1.4426430857935,93.5693692382941));
#9796=CARTESIAN_POINT('Ctrl Pts',(-1.52332772341475,1.29364010344176,93.5813887261374));
#9797=CARTESIAN_POINT('Ctrl Pts',(-1.59982355324681,1.19773213210311,93.5884097664221));
#9798=CARTESIAN_POINT('Ctrl Pts',(-1.66701733785596,1.09548197510851,93.5957235785224));
#9799=CARTESIAN_POINT('Origin',(0.,0.,89.2710285354474));
#9800=CARTESIAN_POINT('',(-1.66701720848889,1.09548217196899,94.5531952825684));
#9801=CARTESIAN_POINT('',(-1.66701746607046,1.09548178000185,94.3957559446131));
#9802=CARTESIAN_POINT('',(-1.66701720851066,1.09548217193587,89.2710285354474));
#9803=CARTESIAN_POINT('',(-1.99474905761762,0.00184918920886758,93.8294109563595));
#9804=CARTESIAN_POINT('Ctrl Pts',(-1.66701720848889,1.09548217196899,94.5531952825684));
#9805=CARTESIAN_POINT('Ctrl Pts',(-1.65877814536531,1.10801971969024,94.5522588550472));
#9806=CARTESIAN_POINT('Ctrl Pts',(-1.65039747779998,1.12046456721701,94.5513305262315));
#9807=CARTESIAN_POINT('Ctrl Pts',(-1.62450307492538,1.15799535947798,94.5485306443866));
#9808=CARTESIAN_POINT('Ctrl Pts',(-1.60655150988994,1.18277467219681,94.5466816763493));
#9809=CARTESIAN_POINT('Ctrl Pts',(-1.54192739585364,1.26779055836618,94.5402998219996));
#9810=CARTESIAN_POINT('Ctrl Pts',(-1.49237836509429,1.32576058053032,94.5358774212361));
#9811=CARTESIAN_POINT('Ctrl Pts',(-1.35242075810157,1.47168597577157,94.5241523801242));
#9812=CARTESIAN_POINT('Ctrl Pts',(-1.25679984611073,1.55414027442987,94.5168661992516));
#9813=CARTESIAN_POINT('Ctrl Pts',(-1.12373179260989,1.64852531373329,94.5069613783697));
#9814=CARTESIAN_POINT('Ctrl Pts',(-1.09282411206984,1.6691746583652,94.5046773719786));
#9815=CARTESIAN_POINT('Ctrl Pts',(-1.04065981086558,1.70195545906256,94.5008374096396));
#9816=CARTESIAN_POINT('Ctrl Pts',(-1.01972388302515,1.71458109855253,94.4993001165723));
#9817=CARTESIAN_POINT('Ctrl Pts',(-0.977448590663658,1.73902750166448,94.4962005553139));
#9818=CARTESIAN_POINT('Ctrl Pts',(-0.956113931721415,1.75084792622617,94.4946386213168));
#9819=CARTESIAN_POINT('Ctrl Pts',(-0.902020836293087,1.77953456532363,94.4906815735246));
#9820=CARTESIAN_POINT('Ctrl Pts',(-0.869002998235498,1.79588929166821,94.4882689682843));
#9821=CARTESIAN_POINT('Ctrl Pts',(-0.741125540299473,1.85487854702981,94.4789299417245));
#9822=CARTESIAN_POINT('Ctrl Pts',(-0.643448962027013,1.89098114233389,94.4717953999255));
#9823=CARTESIAN_POINT('Ctrl Pts',(-0.415370962582188,1.95555733245835,94.4553035478323));
#9824=CARTESIAN_POINT('Ctrl Pts',(-0.284012913178147,1.97890835156229,94.4459159151652));
#9825=CARTESIAN_POINT('Ctrl Pts',(-0.129319918189096,1.99067574956653,94.4355571500884));
#9826=CARTESIAN_POINT('Ctrl Pts',(-0.107310257357126,1.99198348078666,94.434100220218));
#9827=CARTESIAN_POINT('Ctrl Pts',(-0.0728068789317379,1.99345996790867,
94.431847340437));
#9828=CARTESIAN_POINT('Ctrl Pts',(-0.0603261957933327,1.99387669081826,
94.4310387813376));
#9829=CARTESIAN_POINT('Ctrl Pts',(-0.0334924276918565,1.9945204555676,94.4293152109124));
#9830=CARTESIAN_POINT('Ctrl Pts',(-0.0191390545645032,1.9947098329248,94.4284023736306));
#9831=CARTESIAN_POINT('Ctrl Pts',(0.0198136761772904,1.99480326035947,94.4259467423169));
#9832=CARTESIAN_POINT('Ctrl Pts',(0.0444120141936166,1.9944072630241,94.4244194641022));
#9833=CARTESIAN_POINT('Ctrl Pts',(0.152124506610376,1.99067927822345,94.4178099068501));
#9834=CARTESIAN_POINT('Ctrl Pts',(0.234998195084644,1.9826054578836,94.4129265939112));
#9835=CARTESIAN_POINT('Ctrl Pts',(0.46996000404195,1.94476914667243,94.399078874414));
#9836=CARTESIAN_POINT('Ctrl Pts',(0.619389079980499,1.9024570274418,94.3902262158612));
#9837=CARTESIAN_POINT('Ctrl Pts',(0.794031674106413,1.83022169896995,94.3787026051903));
#9838=CARTESIAN_POINT('Ctrl Pts',(0.825299480243103,1.81633651024285,94.3765927251096));
#9839=CARTESIAN_POINT('Ctrl Pts',(0.877600802071935,1.79148155605093,94.3729744300148));
#9840=CARTESIAN_POINT('Ctrl Pts',(0.898824337046323,1.78092786665713,94.3714806032605));
#9841=CARTESIAN_POINT('Ctrl Pts',(0.942026555636191,1.75847602375361,94.3683841977219));
#9842=CARTESIAN_POINT('Ctrl Pts',(0.96397967403659,1.74653801882003,94.3667803973395));
#9843=CARTESIAN_POINT('Ctrl Pts',(1.0205878962206,1.71436230817635,94.3625622762207));
#9844=CARTESIAN_POINT('Ctrl Pts',(1.05486530273371,1.69348651795838,94.3599253520937));
#9845=CARTESIAN_POINT('Ctrl Pts',(1.19618300106117,1.60146492012662,94.3486942095417));
#9846=CARTESIAN_POINT('Ctrl Pts',(1.29683478037455,1.52110303558176,94.3397730302349));
#9847=CARTESIAN_POINT('Ctrl Pts',(1.45783728687042,1.36489017899323,94.3241170658233));
#9848=CARTESIAN_POINT('Ctrl Pts',(1.52173401535396,1.29326839804365,94.3174307016422));
#9849=CARTESIAN_POINT('Ctrl Pts',(1.59569138049773,1.19726267587847,94.309294325021));
#9850=CARTESIAN_POINT('Ctrl Pts',(1.61076349197795,1.17690696828544,94.3076126603283));
#9851=CARTESIAN_POINT('Ctrl Pts',(1.63385013665638,1.14445251828961,94.3050057927724));
#9852=CARTESIAN_POINT('Ctrl Pts',(1.64212683511803,1.13254462373975,94.3040645895399));
#9853=CARTESIAN_POINT('Ctrl Pts',(1.65818987186635,1.10888796523642,94.3022263715666));
#9854=CARTESIAN_POINT('Ctrl Pts',(1.66598291995116,1.09714497764926,94.3013289986563));
#9855=CARTESIAN_POINT('Ctrl Pts',(1.68633087466789,1.06576679047973,94.2989681730435));
#9856=CARTESIAN_POINT('Ctrl Pts',(1.69866769458293,1.04599179972339,94.2975182207548));
#9857=CARTESIAN_POINT('Ctrl Pts',(1.72584954932471,1.0006715194403,94.2942693609485));
#9858=CARTESIAN_POINT('Ctrl Pts',(1.740479529708,0.975003248315662,94.292481236487));
#9859=CARTESIAN_POINT('Ctrl Pts',(1.78850253994539,0.886218830395893,94.2864389506135));
#9860=CARTESIAN_POINT('Ctrl Pts',(1.81907630182492,0.821637224234635,94.2822834492804));
#9861=CARTESIAN_POINT('Ctrl Pts',(1.89688761394112,0.631512362308087,94.2703635230671));
#9862=CARTESIAN_POINT('Ctrl Pts',(1.93501811058044,0.502684357809222,94.2626381646091));
#9863=CARTESIAN_POINT('Ctrl Pts',(1.96676344618634,0.334983058620699,94.2522686357913));
#9864=CARTESIAN_POINT('Ctrl Pts',(1.97258839314024,0.298775621890827,94.2500139112907));
#9865=CARTESIAN_POINT('Ctrl Pts',(1.98061657781982,0.238283168243984,94.2462089969451));
#9866=CARTESIAN_POINT('Ctrl Pts',(1.98337850050852,0.214080675691126,94.2446767185164));
#9867=CARTESIAN_POINT('Ctrl Pts',(1.98802608555792,0.165466263185176,94.2415760371739));
#9868=CARTESIAN_POINT('Ctrl Pts',(1.98990685970579,0.141058151383069,94.2400077613994));
#9869=CARTESIAN_POINT('Ctrl Pts',(1.99352130748105,0.0793411754075412,94.236010774918));
#9870=CARTESIAN_POINT('Ctrl Pts',(1.99465717066892,0.0420081592897301,94.2335638165659));
#9871=CARTESIAN_POINT('Ctrl Pts',(1.99499708561107,-0.103268839732908,94.2239230815013));
#9872=CARTESIAN_POINT('Ctrl Pts',(1.98648864865558,-0.211032967510561,94.2165037350097));
#9873=CARTESIAN_POINT('Ctrl Pts',(1.94914056120583,-0.44263787315862,94.2001670206954));
#9874=CARTESIAN_POINT('Ctrl Pts',(1.91710175250023,-0.565510451063959,94.1912467239069));
#9875=CARTESIAN_POINT('Ctrl Pts',(1.86581140866124,-0.705899029901706,94.1812540631847));
#9876=CARTESIAN_POINT('Ctrl Pts',(1.85763475115789,-0.727144339953264,94.1797481352418));
#9877=CARTESIAN_POINT('Ctrl Pts',(1.84436548688519,-0.759935879159465,94.1774386268102));
#9878=CARTESIAN_POINT('Ctrl Pts',(1.83952425092934,-0.771580936092235,94.1766214206556));
#9879=CARTESIAN_POINT('Ctrl Pts',(1.82900684205424,-0.79621762195198,94.1749000183802));
#9880=CARTESIAN_POINT('Ctrl Pts',(1.82330194091378,-0.809196259719386,94.1739977111454));
#9881=CARTESIAN_POINT('Ctrl Pts',(1.80768173545641,-0.8437280939436,94.1716062715789));
#9882=CARTESIAN_POINT('Ctrl Pts',(1.79751916363818,-0.8651678023182,94.1701312835946));
#9883=CARTESIAN_POINT('Ctrl Pts',(1.77352717224698,-0.913534272911786,94.1668148256097));
#9884=CARTESIAN_POINT('Ctrl Pts',(1.75946238013835,-0.940338137389606,94.1649848262875));
#9885=CARTESIAN_POINT('Ctrl Pts',(1.70860206065416,-1.0321249826431,94.1587105323954));
#9886=CARTESIAN_POINT('Ctrl Pts',(1.66877093169261,-1.0953573949966,94.1543729171989));
#9887=CARTESIAN_POINT('Ctrl Pts',(1.55104574932368,-1.26086414296275,94.1425933259141));
#9888=CARTESIAN_POINT('Ctrl Pts',(1.46668027507267,-1.35807457368512,94.1351738647117));
#9889=CARTESIAN_POINT('Ctrl Pts',(1.34669021923759,-1.47201430151598,94.1251263210794));
#9890=CARTESIAN_POINT('Ctrl Pts',(1.31911521311274,-1.49677501165304,94.1228488146139));
#9891=CARTESIAN_POINT('Ctrl Pts',(1.27224504856193,-1.53656005292961,94.1190166395278));
#9892=CARTESIAN_POINT('Ctrl Pts',(1.25333406638924,-1.55202380542538,94.1174804661503));
#9893=CARTESIAN_POINT('Ctrl Pts',(1.21496836525932,-1.58223740835474,94.1143807034539));
#9894=CARTESIAN_POINT('Ctrl Pts',(1.19551736795742,-1.59698512201632,94.1128174029695));
#9895=CARTESIAN_POINT('Ctrl Pts',(1.14595262606596,-1.63315200455973,94.1088517277386));
#9896=CARTESIAN_POINT('Ctrl Pts',(1.11550626593893,-1.65409744568524,94.1064316989168));
#9897=CARTESIAN_POINT('Ctrl Pts',(0.996514443340254,-1.73117756850181,94.0970283746854));
#9898=CARTESIAN_POINT('Ctrl Pts',(0.904187332282916,-1.78113916536057,94.0898333081222));
#9899=CARTESIAN_POINT('Ctrl Pts',(0.687968751104798,-1.87698507490708,94.073375125702));
#9900=CARTESIAN_POINT('Ctrl Pts',(0.562566625708487,-1.91830571956047,94.0640880254416));
#9901=CARTESIAN_POINT('Ctrl Pts',(0.412331946076651,-1.95179476441778,94.0538076723575));
#9902=CARTESIAN_POINT('Ctrl Pts',(0.390582774671034,-1.95626318067689,94.0523401398014));
#9903=CARTESIAN_POINT('Ctrl Pts',(0.356464878494291,-1.9626810578659,94.050075027217));
#9904=CARTESIAN_POINT('Ctrl Pts',(0.344145366749343,-1.96487865595286,94.0492646208273));
#9905=CARTESIAN_POINT('Ctrl Pts',(0.317692205954323,-1.96934102683323,94.0475417005943));
#9906=CARTESIAN_POINT('Ctrl Pts',(0.30355310205298,-1.97156992325673,94.0466312944225));
#9907=CARTESIAN_POINT('Ctrl Pts',(0.265251805654981,-1.97718594380987,94.0441904253263));
#9908=CARTESIAN_POINT('Ctrl Pts',(0.241048713215539,-1.98028240924477,94.0426751605065));
#9909=CARTESIAN_POINT('Ctrl Pts',(0.135824066286911,-1.99178659100132,94.0361812612194));
#9910=CARTESIAN_POINT('Ctrl Pts',(0.0543800288674653,-1.9956721643413,94.0313936434756));
#9911=CARTESIAN_POINT('Ctrl Pts',(-0.184960421726489,-1.99242262696403,
94.0174584547268));
#9912=CARTESIAN_POINT('Ctrl Pts',(-0.342012742189479,-1.97154299114936,
94.0084390653217));
#9913=CARTESIAN_POINT('Ctrl Pts',(-0.527671360217766,-1.92398827556405,
93.9967452621222));
#9914=CARTESIAN_POINT('Ctrl Pts',(-0.560165202110039,-1.91478006216783,
93.9946612325277));
#9915=CARTESIAN_POINT('Ctrl Pts',(-0.614974763371199,-1.89773341383098,
93.9910731646538));
#9916=CARTESIAN_POINT('Ctrl Pts',(-0.63741392819908,-1.89031464998026,93.9895830961079));
#9917=CARTESIAN_POINT('Ctrl Pts',(-0.683416273752857,-1.87419328963735,
93.9864819012364));
#9918=CARTESIAN_POINT('Ctrl Pts',(-0.706957379123901,-1.86544082143876,
93.9848693262261));
#9919=CARTESIAN_POINT('Ctrl Pts',(-0.768303628899785,-1.84130460565617,
93.9805968106557));
#9920=CARTESIAN_POINT('Ctrl Pts',(-0.805811151358889,-1.82520166058388,
93.9779131484791));
#9921=CARTESIAN_POINT('Ctrl Pts',(-0.889028745586847,-1.78640906990593,
93.9717932221061));
#9922=CARTESIAN_POINT('Ctrl Pts',(-0.934414251957977,-1.76309353312745,
93.9683385408809));
#9923=CARTESIAN_POINT('Ctrl Pts',(-1.10837674595844,-1.66512036997281,93.9546522514962));
#9924=CARTESIAN_POINT('Ctrl Pts',(-1.22933022848395,-1.57793164990642,93.9441092151829));
#9925=CARTESIAN_POINT('Ctrl Pts',(-1.36862307789195,-1.45170451731197,93.9312687216011));
#9926=CARTESIAN_POINT('Ctrl Pts',(-1.39698799277902,-1.42442975580955,93.9286144656591));
#9927=CARTESIAN_POINT('Ctrl Pts',(-1.43672904898935,-1.38388616941381,93.9248600329928));
#9928=CARTESIAN_POINT('Ctrl Pts',(-1.44876545415989,-1.37128042375902,93.9237179558235));
#9929=CARTESIAN_POINT('Ctrl Pts',(-1.46968834420685,-1.34878479429032,93.9217264015465));
#9930=CARTESIAN_POINT('Ctrl Pts',(-1.47864345874466,-1.338961463559,93.9208720849971));
#9931=CARTESIAN_POINT('Ctrl Pts',(-1.49891346599327,-1.31627482064861,93.9189338255884));
#9932=CARTESIAN_POINT('Ctrl Pts',(-1.51016185228887,-1.30335421531302,93.9178545837748));
#9933=CARTESIAN_POINT('Ctrl Pts',(-1.54730230578337,-1.25956587370218,93.9142723223722));
#9934=CARTESIAN_POINT('Ctrl Pts',(-1.57242694269054,-1.2280572468943,93.9118175118612));
#9935=CARTESIAN_POINT('Ctrl Pts',(-1.63609156501138,-1.14305542888454,93.9054468966782));
#9936=CARTESIAN_POINT('Ctrl Pts',(-1.67296514493075,-1.08837491582328,93.9015976883592));
#9937=CARTESIAN_POINT('Ctrl Pts',(-1.78201946006359,-0.907978650159301,
93.8893512695102));
#9938=CARTESIAN_POINT('Ctrl Pts',(-1.84323582364829,-0.776206364462101,
93.8810340427052));
#9939=CARTESIAN_POINT('Ctrl Pts',(-1.90099129240392,-0.605404954737159,
93.8700605206674));
#9940=CARTESIAN_POINT('Ctrl Pts',(-1.91144443599477,-0.57154438392123,93.8678784987383));
#9941=CARTESIAN_POINT('Ctrl Pts',(-1.92742971719943,-0.514406053835909,
93.864175195573));
#9942=CARTESIAN_POINT('Ctrl Pts',(-1.93345507876547,-0.491274140584253,
93.8626702634296));
#9943=CARTESIAN_POINT('Ctrl Pts',(-1.94485432327511,-0.444047751229549,
93.8595835123776));
#9944=CARTESIAN_POINT('Ctrl Pts',(-1.95019949184321,-0.419950705610756,
93.858001058756));
#9945=CARTESIAN_POINT('Ctrl Pts',(-1.96008624682162,-0.371109289120179,
93.8547766195633));
#9946=CARTESIAN_POINT('Ctrl Pts',(-1.96460958394189,-0.346365827303723,
93.8531343674238));
#9947=CARTESIAN_POINT('Ctrl Pts',(-1.97499847301754,-0.282759583788984,
93.8488891054048));
#9948=CARTESIAN_POINT('Ctrl Pts',(-1.9801853328603,-0.243798393516646,93.84626611072));
#9949=CARTESIAN_POINT('Ctrl Pts',(-1.99129863967524,-0.136079862540772,
93.838953796603));
#9950=CARTESIAN_POINT('Ctrl Pts',(-1.99481311978167,-0.067133567392285,
93.8342045185029));
#9951=CARTESIAN_POINT('Ctrl Pts',(-1.99474914212584,0.00184999681506738,
93.8294110481131));
#9952=CARTESIAN_POINT('Ctrl Pts',(-1.99474914286513,0.00184919951270623,
93.8294111035154));
#9953=CARTESIAN_POINT('Ctrl Pts',(-1.99462397475624,0.136869231801161,93.8200289485989));
#9954=CARTESIAN_POINT('Ctrl Pts',(-1.98079066454154,0.271536840527291,93.8104912318438));
#9955=CARTESIAN_POINT('Ctrl Pts',(-1.94859746654462,0.427283678473688,93.7998361128864));
#9956=CARTESIAN_POINT('Ctrl Pts',(-1.94331593803251,0.450695813799839,93.7982455201724));
#9957=CARTESIAN_POINT('Ctrl Pts',(-1.93423114022538,0.48783193030372,93.795746305063));
#9958=CARTESIAN_POINT('Ctrl Pts',(-1.93070137826948,0.501619693313766,93.7948236788762));
#9959=CARTESIAN_POINT('Ctrl Pts',(-1.9237767885384,0.527511531704006,93.7931025842245));
#9960=CARTESIAN_POINT('Ctrl Pts',(-1.92041456497507,0.539623449765512,93.7923022311904));
#9961=CARTESIAN_POINT('Ctrl Pts',(-1.91070800480892,0.573349690034312,93.7900848293567));
#9962=CARTESIAN_POINT('Ctrl Pts',(-1.90411151867594,0.594890218949912,93.7886815402064));
#9963=CARTESIAN_POINT('Ctrl Pts',(-1.85735859713285,0.738805748324284,93.7793644012841));
#9964=CARTESIAN_POINT('Ctrl Pts',(-1.80579145843149,0.857169984270223,93.7719734846332));
#9965=CARTESIAN_POINT('Ctrl Pts',(-1.71932457295764,1.01259823602324,93.7616551244413));
#9966=CARTESIAN_POINT('Ctrl Pts',(-1.69392384772003,1.0545378050329,93.7588051545207));
#9967=CARTESIAN_POINT('Ctrl Pts',(-1.66701713450993,1.09548228454426,93.7559248887299));
#9968=CARTESIAN_POINT('',(-1.99475046548998,-0.00047329462618507,93.6728333695482));
#9969=CARTESIAN_POINT('Ctrl Pts',(-1.66701733785596,1.09548197510851,93.5957235785224));
#9970=CARTESIAN_POINT('Ctrl Pts',(-1.68382990952458,1.06989794077261,93.5975535690613));
#9971=CARTESIAN_POINT('Ctrl Pts',(-1.70006015033342,1.04391678375076,93.5994006921208));
#9972=CARTESIAN_POINT('Ctrl Pts',(-1.73325899504351,0.987940554734956,93.6033675317161));
#9973=CARTESIAN_POINT('Ctrl Pts',(-1.75005382536845,0.957875081423901,93.6054907201682));
#9974=CARTESIAN_POINT('Ctrl Pts',(-1.77709515091515,0.906379408478577,93.6091243008571));
#9975=CARTESIAN_POINT('Ctrl Pts',(-1.78775263093988,0.885173011029849,93.6106197782722));
#9976=CARTESIAN_POINT('Ctrl Pts',(-1.80881826746923,0.841323275402433,93.6137130011928));
#9977=CARTESIAN_POINT('Ctrl Pts',(-1.81918549136577,0.818665030883475,93.6153118489053));
#9978=CARTESIAN_POINT('Ctrl Pts',(-1.84498983427763,0.759355876062686,93.6195008497259));
#9979=CARTESIAN_POINT('Ctrl Pts',(-1.85975953843096,0.722428487904385,93.6221130272067));
#9980=CARTESIAN_POINT('Ctrl Pts',(-1.91791393370979,0.563401383673303,93.6333850330902));
#9981=CARTESIAN_POINT('Ctrl Pts',(-1.950445242861,0.437686318157782,93.6423796064582));
#9982=CARTESIAN_POINT('Ctrl Pts',(-1.98232649146809,0.234849380821766,93.656709282206));
#9983=CARTESIAN_POINT('Ctrl Pts',(-1.98981866226028,0.159359265007278,93.6619961768541));
#9984=CARTESIAN_POINT('Ctrl Pts',(-1.99417188367383,0.0556081062775789,
93.6690725907853));
#9985=CARTESIAN_POINT('Ctrl Pts',(-1.99475656749687,0.0275705606384254,
93.6709656878819));
#9986=CARTESIAN_POINT('Ctrl Pts',(-1.99474994436128,-0.000471137632967747,
93.6728341296312));
#9987=CARTESIAN_POINT('Ctrl Pts',(-1.99474994386491,-0.000473234538596436,
93.6728342693498));
#9988=CARTESIAN_POINT('Ctrl Pts',(-1.99474660187362,-0.0145601965145745,
93.6737728947528));
#9989=CARTESIAN_POINT('Ctrl Pts',(-1.99459403618466,-0.0286472457323476,
93.6747052266267));
#9990=CARTESIAN_POINT('Ctrl Pts',(-1.99399045765822,-0.0568161117758029,
93.6765554132599));
#9991=CARTESIAN_POINT('Ctrl Pts',(-1.99353947529967,-0.0708971409524056,
93.6774732166138));
#9992=CARTESIAN_POINT('Ctrl Pts',(-1.99237775670518,-0.0981439454589759,
93.6792339620626));
#9993=CARTESIAN_POINT('Ctrl Pts',(-1.99168566144922,-0.111308559768748,
93.6800775829642));
#9994=CARTESIAN_POINT('Ctrl Pts',(-1.98965922496718,-0.143721770119643,
93.6821385238247));
#9995=CARTESIAN_POINT('Ctrl Pts',(-1.9881760626398,-0.162959472154204,93.6833478528335));
#9996=CARTESIAN_POINT('Ctrl Pts',(-1.98139508284564,-0.236899064765848,
93.6879528673883));
#9997=CARTESIAN_POINT('Ctrl Pts',(-1.97411636760926,-0.291398798271338,
93.6912566358625));
#9998=CARTESIAN_POINT('Ctrl Pts',(-1.95472287231988,-0.401664396129385,
93.6978798064567));
#9999=CARTESIAN_POINT('Ctrl Pts',(-1.94244894939685,-0.457349248172171,
93.7011923668612));
#10000=CARTESIAN_POINT('Ctrl Pts',(-1.90711040483513,-0.590294996565072,
93.7091719511386));
#10001=CARTESIAN_POINT('Ctrl Pts',(-1.88171632705291,-0.666829332174217,
93.713827281217));
#10002=CARTESIAN_POINT('Ctrl Pts',(-1.8265594919523,-0.804552214992443,
93.7225803402644));
#10003=CARTESIAN_POINT('Ctrl Pts',(-1.79816414114437,-0.866157173060337,
93.7266430927624));
#10004=CARTESIAN_POINT('Ctrl Pts',(-1.75300775377003,-0.952291820612311,
93.7326222817654));
#10005=CARTESIAN_POINT('Ctrl Pts',(-1.73874950995876,-0.978082764812323,
93.7344526506466));
#10006=CARTESIAN_POINT('Ctrl Pts',(-1.71218258699017,-1.02372027363406,
93.737769787191));
#10007=CARTESIAN_POINT('Ctrl Pts',(-1.7000866277015,-1.04368471887101,93.7392486309641));
#10008=CARTESIAN_POINT('Ctrl Pts',(-1.67313813526597,-1.08645140661088,
93.7424796561735));
#10009=CARTESIAN_POINT('Ctrl Pts',(-1.65816390074364,-1.1091709672942,93.7442361861689));
#10010=CARTESIAN_POINT('Ctrl Pts',(-1.61384334494729,-1.17351194140583,
93.7493303283768));
#10011=CARTESIAN_POINT('Ctrl Pts',(-1.58336357099285,-1.21432271588118,
93.7527101165153));
#10012=CARTESIAN_POINT('Ctrl Pts',(-1.45369037090604,-1.37475525703491,
93.7666160268956));
#10013=CARTESIAN_POINT('Ctrl Pts',(-1.34224499953218,-1.48375711668785,
93.7775856899134));
#10014=CARTESIAN_POINT('Ctrl Pts',(-1.18633764710202,-1.60417142408417,
93.7912155777713));
#10015=CARTESIAN_POINT('Ctrl Pts',(-1.15257655720715,-1.62859774914347,
93.7940748744114));
#10016=CARTESIAN_POINT('Ctrl Pts',(-1.09337412027603,-1.66866716884381,
93.7989043867696));
#10017=CARTESIAN_POINT('Ctrl Pts',(-1.06830127082955,-1.68482927983789,
93.8008957614767));
#10018=CARTESIAN_POINT('Ctrl Pts',(-1.02976676801425,-1.70846257858821,
93.8038649023371));
#10019=CARTESIAN_POINT('Ctrl Pts',(-1.01656661326717,-1.71634971283828,
93.8048661821745));
#10020=CARTESIAN_POINT('Ctrl Pts',(-0.991664843150677,-1.7308405114638,
93.8067237339182));
#10021=CARTESIAN_POINT('Ctrl Pts',(-0.97998571558448,-1.73747979637569,
93.8075820481971));
#10022=CARTESIAN_POINT('Ctrl Pts',(-0.950392146728589,-1.75390965119886,
93.8097264586801));
#10023=CARTESIAN_POINT('Ctrl Pts',(-0.93239231513687,-1.76354442690906,
93.811003139794));
#10024=CARTESIAN_POINT('Ctrl Pts',(-0.857933612010118,-1.80194116537811,
93.8161850359675));
#10025=CARTESIAN_POINT('Ctrl Pts',(-0.800263237426656,-1.82828397384793,
93.8199679620237));
#10026=CARTESIAN_POINT('Ctrl Pts',(-0.625710072406765,-1.898170864491,93.8310241635355));
#10027=CARTESIAN_POINT('Ctrl Pts',(-0.505900350255956,-1.93355417388032,
93.8381256182141));
#10028=CARTESIAN_POINT('Ctrl Pts',(-0.336565421072765,-1.96673473501722,
93.8482963851583));
#10029=CARTESIAN_POINT('Ctrl Pts',(-0.289247102256536,-1.97424858662186,
93.8511500261183));
#10030=CARTESIAN_POINT('Ctrl Pts',(-0.202964388590369,-1.98478117734626,
93.8564142697464));
#10031=CARTESIAN_POINT('Ctrl Pts',(-0.164094179975455,-1.98837211168075,
93.858807824392));
#10032=CARTESIAN_POINT('Ctrl Pts',(-0.100413548997051,-1.99237515783081,
93.8627792051893));
#10033=CARTESIAN_POINT('Ctrl Pts',(-0.0756556915753041,-1.99346878029904,
93.864335463143));
#10034=CARTESIAN_POINT('Ctrl Pts',(-0.027072715856891,-1.99470850317478,
93.8674164682595));
#10035=CARTESIAN_POINT('Ctrl Pts',(-0.00325261441307909,-1.99488954166603,
93.868939845437));
#10036=CARTESIAN_POINT('Ctrl Pts',(0.0555289642162972,-1.99428352097563,
93.8727330196911));
#10037=CARTESIAN_POINT('Ctrl Pts',(0.0904762358002397,-1.99300376862146,
93.8750178563666));
#10038=CARTESIAN_POINT('Ctrl Pts',(0.274301034826361,-1.981427490311,93.8871999151269));
#10039=CARTESIAN_POINT('Ctrl Pts',(0.421687035470673,-1.95536741019804,
93.8975850246593));
#10040=CARTESIAN_POINT('Ctrl Pts',(0.625894879735792,-1.89508473915859,
93.9124382178875));
#10041=CARTESIAN_POINT('Ctrl Pts',(0.686131356732233,-1.87411715377668,
93.9168725362948));
#10042=CARTESIAN_POINT('Ctrl Pts',(0.781875085440731,-1.83555354916185,
93.9239168798862));
#10043=CARTESIAN_POINT('Ctrl Pts',(0.818044345055888,-1.81972233848153,
93.9265767369699));
#10044=CARTESIAN_POINT('Ctrl Pts',(0.869091152501267,-1.79554930150296,
93.9303057495643));
#10045=CARTESIAN_POINT('Ctrl Pts',(0.884366808824619,-1.78807497646299,
93.9314183497518));
#10046=CARTESIAN_POINT('Ctrl Pts',(0.911410338073204,-1.77441130083946,
93.9333796991753));
#10047=CARTESIAN_POINT('Ctrl Pts',(0.923214409355658,-1.76829846017705,
93.9342326977994));
#10048=CARTESIAN_POINT('Ctrl Pts',(0.950462070276944,-1.75384078038997,
93.9361949943438));
#10049=CARTESIAN_POINT('Ctrl Pts',(0.965857939541601,-1.74540944260488,
93.9372989989004));
#10050=CARTESIAN_POINT('Ctrl Pts',(1.01608580483633,-1.71703466314968,93.9408916778265));
#10051=CARTESIAN_POINT('Ctrl Pts',(1.05042926877709,-1.69624208518923,93.943333733786));
#10052=CARTESIAN_POINT('Ctrl Pts',(1.20812630889072,-1.59413951647265,93.954590641622));
#10053=CARTESIAN_POINT('Ctrl Pts',(1.32283277100802,-1.50032314931616,93.9629388629905));
#10054=CARTESIAN_POINT('Ctrl Pts',(1.46172589069291,-1.35829908370278,93.9746151731138));
#10055=CARTESIAN_POINT('Ctrl Pts',(1.49591027729057,-1.32055705196346,93.9776389794543));
#10056=CARTESIAN_POINT('Ctrl Pts',(1.55479330926606,-1.25032235008209,93.9831776506486));
#10057=CARTESIAN_POINT('Ctrl Pts',(1.58000971394817,-1.21830093498907,93.9856722626986));
#10058=CARTESIAN_POINT('Ctrl Pts',(1.61914318833425,-1.16534665467781,93.9897657485668));
#10059=CARTESIAN_POINT('Ctrl Pts',(1.63367693174514,-1.14488299872273,93.9913402502351));
#10060=CARTESIAN_POINT('Ctrl Pts',(1.66113717488308,-1.10463081599153,93.9944264234733));
#10061=CARTESIAN_POINT('Ctrl Pts',(1.67410572826589,-1.08487597650066,93.9959361358999));
#10062=CARTESIAN_POINT('Ctrl Pts',(1.7047572779801,-1.0363260972633,93.9996370081963));
#10063=CARTESIAN_POINT('Ctrl Pts',(1.72206492551498,-1.00730398427055,94.0018415459047));
#10064=CARTESIAN_POINT('Ctrl Pts',(1.81596340937894,-0.84035293288418,94.0144875508056));
#10065=CARTESIAN_POINT('Ctrl Pts',(1.87670291423943,-0.694179647501685,
94.0254885712474));
#10066=CARTESIAN_POINT('Ctrl Pts',(1.94175888886326,-0.463948780345325,
94.0421682492272));
#10067=CARTESIAN_POINT('Ctrl Pts',(1.95910079833111,-0.384190465057437,
94.0478226945815));
#10068=CARTESIAN_POINT('Ctrl Pts',(1.97522663671268,-0.279468885810256,
94.0549261084285));
#10069=CARTESIAN_POINT('Ctrl Pts',(1.97849805899632,-0.255281577539669,
94.0565446128269));
#10070=CARTESIAN_POINT('Ctrl Pts',(1.98298256808391,-0.216823709869348,
94.059076691998));
#10071=CARTESIAN_POINT('Ctrl Pts',(1.98448722595458,-0.20259039251445,94.0600048729891));
#10072=CARTESIAN_POINT('Ctrl Pts',(1.987019541698,-0.175890127427713,94.0617277494856));
#10073=CARTESIAN_POINT('Ctrl Pts',(1.98808336972325,-0.163427447081837,
94.0625244646784));
#10074=CARTESIAN_POINT('Ctrl Pts',(1.99070843843327,-0.128838772818492,
94.0647170305938));
#10075=CARTESIAN_POINT('Ctrl Pts',(1.99201803098366,-0.10669478803277,94.0660996362109));
#10076=CARTESIAN_POINT('Ctrl Pts',(1.99854585342463,0.0472067020327452,
94.0755909836437));
#10077=CARTESIAN_POINT('Ctrl Pts',(1.99105823810366,0.179192468372397,94.0831471717682));
#10078=CARTESIAN_POINT('Ctrl Pts',(1.95434646639441,0.412947503039959,94.096877911222));
#10079=CARTESIAN_POINT('Ctrl Pts',(1.92997687187872,0.514958318723832,94.1029937156257));
#10080=CARTESIAN_POINT('Ctrl Pts',(1.88633522565453,0.649716131997069,94.1115962649241));
#10081=CARTESIAN_POINT('Ctrl Pts',(1.87398307316575,0.684528166074212,94.1138665942333));
#10082=CARTESIAN_POINT('Ctrl Pts',(1.85187751695145,0.741736217348781,94.1176898594097));
#10083=CARTESIAN_POINT('Ctrl Pts',(1.84266614439187,0.764332616874433,94.1192244790452));
#10084=CARTESIAN_POINT('Ctrl Pts',(1.82341094472551,0.80919495744426,94.1223235603189));
#10085=CARTESIAN_POINT('Ctrl Pts',(1.8133680430868,0.831456676394288,94.12388777873));
#10086=CARTESIAN_POINT('Ctrl Pts',(1.78706699842629,0.887012772082696,94.1278608872834));
#10087=CARTESIAN_POINT('Ctrl Pts',(1.77028581895735,0.92004778655433,94.1302875834516));
#10088=CARTESIAN_POINT('Ctrl Pts',(1.69124175549195,1.06547403385005,94.141267226823));
#10089=CARTESIAN_POINT('Ctrl Pts',(1.61913500289807,1.17214597465599,94.1501594368165));
#10090=CARTESIAN_POINT('Ctrl Pts',(1.48971703785157,1.32866236186849,94.164331767512));
#10091=CARTESIAN_POINT('Ctrl Pts',(1.43895183055248,1.38348075864037,94.1695474173394));
#10092=CARTESIAN_POINT('Ctrl Pts',(1.36345894261606,1.45633885224281,94.176730939166));
#10093=CARTESIAN_POINT('Ctrl Pts',(1.34120993733703,1.4768545049761,94.1787844058516));
#10094=CARTESIAN_POINT('Ctrl Pts',(1.30070335310181,1.51253460099505,94.1823992458531));
#10095=CARTESIAN_POINT('Ctrl Pts',(1.2826258261464,1.5278943816045,94.1839707406079));
#10096=CARTESIAN_POINT('Ctrl Pts',(1.25331526857232,1.55191148680318,94.1864472110057));
#10097=CARTESIAN_POINT('Ctrl Pts',(1.24225693369214,1.56077742511963,94.1873657864092));
#10098=CARTESIAN_POINT('Ctrl Pts',(1.22118572201773,1.5773052681468,94.1890850701671));
#10099=CARTESIAN_POINT('Ctrl Pts',(1.21119302545486,1.58499146765078,94.1898875683919));
#10100=CARTESIAN_POINT('Ctrl Pts',(1.18296475799256,1.60628126169809,94.1921208930795));
#10101=CARTESIAN_POINT('Ctrl Pts',(1.16456777383121,1.61966882870458,94.1935376195694));
#10102=CARTESIAN_POINT('Ctrl Pts',(1.04219267490347,1.7055582964341,94.2027390201555));
#10103=CARTESIAN_POINT('Ctrl Pts',(0.931722647487114,1.76833127626115,94.2100198962002));
#10104=CARTESIAN_POINT('Ctrl Pts',(0.717582925363837,1.86433421530465,94.2236322613004));
#10105=CARTESIAN_POINT('Ctrl Pts',(0.615727053153437,1.90040639267756,94.2299212430756));
#10106=CARTESIAN_POINT('Ctrl Pts',(0.475372728777888,1.93763831568532,94.2387351459183));
#10107=CARTESIAN_POINT('Ctrl Pts',(0.43902602604148,1.94619560862729,94.2410291078333));
#10108=CARTESIAN_POINT('Ctrl Pts',(0.378493014018842,1.95866523641376,94.2448806889106));
#10109=CARTESIAN_POINT('Ctrl Pts',(0.354435782124617,1.96316113975725,94.2464193819229));
#10110=CARTESIAN_POINT('Ctrl Pts',(0.306287980925508,1.97124534322307,94.2495177548893));
#10111=CARTESIAN_POINT('Ctrl Pts',(0.282202317599193,1.97483728318786,94.2510770270853));
#10112=CARTESIAN_POINT('Ctrl Pts',(0.221711923730755,1.98272915266453,94.2550189041925));
#10113=CARTESIAN_POINT('Ctrl Pts',(0.185244417643904,1.98646804170269,94.2574187271263));
#10114=CARTESIAN_POINT('Ctrl Pts',(0.0537425722199683,1.99629805712961,
94.2661614256868));
#10115=CARTESIAN_POINT('Ctrl Pts',(-0.0415858162103165,1.99658726086145,
94.2726734217836));
#10116=CARTESIAN_POINT('Ctrl Pts',(-0.265009734361744,1.98125579170285,
94.2882217314387));
#10117=CARTESIAN_POINT('Ctrl Pts',(-0.392306789321386,1.96002603095119,
94.2973125324171));
#10118=CARTESIAN_POINT('Ctrl Pts',(-0.545321495904473,1.91899239750081,
94.3080128319002));
#10119=CARTESIAN_POINT('Ctrl Pts',(-0.573797441173737,1.91067110436594,
94.3099929229632));
#10120=CARTESIAN_POINT('Ctrl Pts',(-0.616708338418779,1.89708562312931,
94.3129489716658));
#10121=CARTESIAN_POINT('Ctrl Pts',(-0.631284456391861,1.89228512864927,
94.3139481499711));
#10122=CARTESIAN_POINT('Ctrl Pts',(-0.6585252827618,1.88296383021898,94.3158042671725));
#10123=CARTESIAN_POINT('Ctrl Pts',(-0.671201892513914,1.87848246245331,
94.3166632005401));
#10124=CARTESIAN_POINT('Ctrl Pts',(-0.703076964403794,1.86685029177569,
94.3188126363815));
#10125=CARTESIAN_POINT('Ctrl Pts',(-0.722212937587476,1.85953106485829,
94.3200936224265));
#10126=CARTESIAN_POINT('Ctrl Pts',(-0.805697204827674,1.82611633087875,
94.3256548311249));
#10127=CARTESIAN_POINT('Ctrl Pts',(-0.868776220092474,1.79696372066087,
94.3297856004103));
#10128=CARTESIAN_POINT('Ctrl Pts',(-1.03635689587212,1.70862218497011,94.3408921083088));
#10129=CARTESIAN_POINT('Ctrl Pts',(-1.13723611467703,1.64320418712213,94.3477399635334));
#10130=CARTESIAN_POINT('Ctrl Pts',(-1.268728526189,1.53999358369181,94.3575999267126));
#10131=CARTESIAN_POINT('Ctrl Pts',(-1.304784793124,1.50956567819077,94.3604121429735));
#10132=CARTESIAN_POINT('Ctrl Pts',(-1.36832824530758,1.45196267621233,94.3656092001478));
#10133=CARTESIAN_POINT('Ctrl Pts',(-1.39616900729853,1.42521212514782,94.3679777324168));
#10134=CARTESIAN_POINT('Ctrl Pts',(-1.44052346478258,1.38004707743838,94.3719189529604));
#10135=CARTESIAN_POINT('Ctrl Pts',(-1.45750252326476,1.36210282112052,94.3734707479523));
#10136=CARTESIAN_POINT('Ctrl Pts',(-1.49022765095059,1.32620477895533,94.3765510681031));
#10137=CARTESIAN_POINT('Ctrl Pts',(-1.5059932432108,1.30827437357928,94.3780783771192));
#10138=CARTESIAN_POINT('Ctrl Pts',(-1.54426016921174,1.26314447034638,94.3818974987313));
#10139=CARTESIAN_POINT('Ctrl Pts',(-1.56636778168429,1.23562337772486,94.3842048245139));
#10140=CARTESIAN_POINT('Ctrl Pts',(-1.61545779480429,1.17107698714966,94.3895708216905));
#10141=CARTESIAN_POINT('Ctrl Pts',(-1.64189998476113,1.13370357502457,94.3926453687346));
#10142=CARTESIAN_POINT('Ctrl Pts',(-1.66701746607045,1.09548178000186,94.3957559446131));
#10143=CARTESIAN_POINT('Origin',(0.,0.,89.2710285354474));
#10144=CARTESIAN_POINT('',(-1.66701714412027,1.09548226992002,95.3554060137221));
#10145=CARTESIAN_POINT('',(-1.66701720893993,1.09548217128264,95.1987207124569));
#10146=CARTESIAN_POINT('',(-1.66701720851066,1.09548217193587,89.2710285354474));
#10147=CARTESIAN_POINT('Ctrl Pts',(-1.66701714412024,1.09548226992006,95.3554060137221));
#10148=CARTESIAN_POINT('Ctrl Pts',(-1.64000640050892,1.13658505534331,95.3519840620999));
#10149=CARTESIAN_POINT('Ctrl Pts',(-1.61146537971087,1.17670425752475,95.3485433737237));
#10150=CARTESIAN_POINT('Ctrl Pts',(-1.53292208075897,1.27887297180187,95.3395615817572));
#10151=CARTESIAN_POINT('Ctrl Pts',(-1.48065870255216,1.3390362592318,95.3340455315168));
#10152=CARTESIAN_POINT('Ctrl Pts',(-1.40801552310433,1.41318944202132,95.3270887724191));
#10153=CARTESIAN_POINT('Ctrl Pts',(-1.39078269325614,1.43015234785357,95.3254858138427));
#10154=CARTESIAN_POINT('Ctrl Pts',(-1.36289667472665,1.45662066896006,95.322972014917));
#10155=CARTESIAN_POINT('Ctrl Pts',(-1.35244305211034,1.46633179783612,95.3220469045316));
#10156=CARTESIAN_POINT('Ctrl Pts',(-1.33260507548917,1.48436808178,95.3203249220826));
#10157=CARTESIAN_POINT('Ctrl Pts',(-1.32324473203996,1.49271842259496,95.3195261043901));
#10158=CARTESIAN_POINT('Ctrl Pts',(-1.29697036202853,1.51571634336574,95.3173195269075));
#10159=CARTESIAN_POINT('Ctrl Pts',(-1.2798872036958,1.53016894458555,95.3159253000714));
#10160=CARTESIAN_POINT('Ctrl Pts',(-1.16180158695774,1.62670947545258,95.3065309272179));
#10161=CARTESIAN_POINT('Ctrl Pts',(-1.05320615018574,1.69903854536474,95.2990667087308));
#10162=CARTESIAN_POINT('Ctrl Pts',(-0.844981353867737,1.81003398973017,
95.285376251291));
#10163=CARTESIAN_POINT('Ctrl Pts',(-0.747836220846204,1.85228359813868,
95.2792028864927));
#10164=CARTESIAN_POINT('Ctrl Pts',(-0.61274129340497,1.89867061105845,95.2705297819906));
#10165=CARTESIAN_POINT('Ctrl Pts',(-0.577350616843583,1.90972981788722,
95.2682512161602));
#10166=CARTESIAN_POINT('Ctrl Pts',(-0.518160901684755,1.92643030548239,
95.2644177399511));
#10167=CARTESIAN_POINT('Ctrl Pts',(-0.494528792083287,1.93263178862709,
95.2628813510899));
#10168=CARTESIAN_POINT('Ctrl Pts',(-0.44707260379844,1.94415774161554,95.2597815261279));
#10169=CARTESIAN_POINT('Ctrl Pts',(-0.423252849652262,1.94948202728075,
95.2582183857543));
#10170=CARTESIAN_POINT('Ctrl Pts',(-0.363154823951822,1.96176205030644,
95.2542538868453));
#10171=CARTESIAN_POINT('Ctrl Pts',(-0.32677116801332,1.96814940243149,95.2518348981535));
#10172=CARTESIAN_POINT('Ctrl Pts',(-0.161170245646818,1.99250324752168,
95.2407334857278));
#10173=CARTESIAN_POINT('Ctrl Pts',(-0.0305751668670882,1.99877476163169,
95.2316992618598));
#10174=CARTESIAN_POINT('Ctrl Pts',(0.173037175092029,1.98858769896971,95.2174721654136));
#10175=CARTESIAN_POINT('Ctrl Pts',(0.246142544232215,1.98086789116589,95.2123424697461));
#10176=CARTESIAN_POINT('Ctrl Pts',(0.348270769375714,1.96434083538861,95.2052611590111));
#10177=CARTESIAN_POINT('Ctrl Pts',(0.377773255114963,1.95888105674249,95.2032260225623));
#10178=CARTESIAN_POINT('Ctrl Pts',(0.430216521192827,1.94794682925256,95.1996394916636));
#10179=CARTESIAN_POINT('Ctrl Pts',(0.453204446764953,1.94272719427836,95.1980781915435));
#10180=CARTESIAN_POINT('Ctrl Pts',(0.489832563574475,1.93372483165117,95.1956135761548));
#10181=CARTESIAN_POINT('Ctrl Pts',(0.503533813988761,1.93020242434779,95.1946968800585));
#10182=CARTESIAN_POINT('Ctrl Pts',(0.531141981485651,1.92279074114548,95.192861926143));
#10183=CARTESIAN_POINT('Ctrl Pts',(0.5450463802842,1.9188956493574,95.1919440307082));
#10184=CARTESIAN_POINT('Ctrl Pts',(0.582922552044203,1.90784032425974,95.1894576664844));
#10185=CARTESIAN_POINT('Ctrl Pts',(0.606804644935765,1.90037934683931,95.1879053828174));
#10186=CARTESIAN_POINT('Ctrl Pts',(0.718287091064494,1.86323515807974,95.1807045866458));
#10187=CARTESIAN_POINT('Ctrl Pts',(0.80390269635338,1.82792930098886,95.1753039603777));
#10188=CARTESIAN_POINT('Ctrl Pts',(0.974086549453968,1.7434694797139,95.16427192238));
#10189=CARTESIAN_POINT('Ctrl Pts',(1.0581113476354,1.69379157978336,95.158655870719));
#10190=CARTESIAN_POINT('Ctrl Pts',(1.18868792745926,1.60306998733783,95.1492343798801));
#10191=CARTESIAN_POINT('Ctrl Pts',(1.23755643119603,1.56565175523927,95.1455322257767));
#10192=CARTESIAN_POINT('Ctrl Pts',(1.30650373206005,1.50761207985663,95.1399814498158));
#10193=CARTESIAN_POINT('Ctrl Pts',(1.32799246049851,1.48871826687761,95.1382014755914));
#10194=CARTESIAN_POINT('Ctrl Pts',(1.36623771251457,1.45360430197288,95.1349360262293));
#10195=CARTESIAN_POINT('Ctrl Pts',(1.38313054452707,1.43753983422498,95.1334573380849));
#10196=CARTESIAN_POINT('Ctrl Pts',(1.41962970835688,1.40159145536372,95.1301788495971));
#10197=CARTESIAN_POINT('Ctrl Pts',(1.43910756775304,1.38158473972121,95.1283737462407));
#10198=CARTESIAN_POINT('Ctrl Pts',(1.49701301251369,1.31955362327645,95.1228316039774));
#10199=CARTESIAN_POINT('Ctrl Pts',(1.53406420810023,1.27628980992534,95.1190385783563));
#10200=CARTESIAN_POINT('Ctrl Pts',(1.66067064850778,1.11496487680025,95.1051490975733));
#10201=CARTESIAN_POINT('Ctrl Pts',(1.73885720476997,0.988605557061351,95.0946895564644));
#10202=CARTESIAN_POINT('Ctrl Pts',(1.81990456802142,0.817714924312398,95.0816091433359));
#10203=CARTESIAN_POINT('Ctrl Pts',(1.83633639577286,0.780114954124258,95.0787950208599));
#10204=CARTESIAN_POINT('Ctrl Pts',(1.86257450586625,0.714642906436793,95.074031853511));
#10205=CARTESIAN_POINT('Ctrl Pts',(1.87294278370813,0.687010783473413,95.0720623495546));
#10206=CARTESIAN_POINT('Ctrl Pts',(1.88775676664163,0.644698859152281,95.0691184266652));
#10207=CARTESIAN_POINT('Ctrl Pts',(1.89265229374907,0.63018216463559,95.0681210629457));
#10208=CARTESIAN_POINT('Ctrl Pts',(1.90153441752246,0.602806443425458,95.0662658162068));
#10209=CARTESIAN_POINT('Ctrl Pts',(1.90555883430308,0.589961258570713,95.0654059860135));
#10210=CARTESIAN_POINT('Ctrl Pts',(1.91540290507772,0.557388787449253,95.0632506806532));
#10211=CARTESIAN_POINT('Ctrl Pts',(1.92104823126789,0.537609822967386,95.0619648335877));
#10212=CARTESIAN_POINT('Ctrl Pts',(1.94477135643207,0.449342791310319,95.0563133417703));
#10213=CARTESIAN_POINT('Ctrl Pts',(1.95950129187206,0.3800016458441,95.052103461659));
#10214=CARTESIAN_POINT('Ctrl Pts',(1.98898019562982,0.192629922334281,95.0409907313784));
#10215=CARTESIAN_POINT('Ctrl Pts',(1.99692223099103,0.0738280114103413,
95.034206047352));
#10216=CARTESIAN_POINT('Ctrl Pts',(1.99318363263276,-0.091944548102242,
95.0244236391947));
#10217=CARTESIAN_POINT('Ctrl Pts',(1.99046539747487,-0.138859211699801,
95.0216219725172));
#10218=CARTESIAN_POINT('Ctrl Pts',(1.98251119776994,-0.223961864711707,
95.0164419218809));
#10219=CARTESIAN_POINT('Ctrl Pts',(1.97782003657836,-0.262177744840459,
95.0140796578135));
#10220=CARTESIAN_POINT('Ctrl Pts',(1.96831060242317,-0.324638926262241,
95.0101456856472));
#10221=CARTESIAN_POINT('Ctrl Pts',(1.96414213997096,-0.348973675619511,
95.0085946977961));
#10222=CARTESIAN_POINT('Ctrl Pts',(1.95505195471309,-0.39669952366313,95.0055136460254));
#10223=CARTESIAN_POINT('Ctrl Pts',(1.95015930732267,-0.420091955768283,
95.0039847553345));
#10224=CARTESIAN_POINT('Ctrl Pts',(1.93697836674742,-0.477907696068513,
95.0001569487279));
#10225=CARTESIAN_POINT('Ctrl Pts',(1.92819187305794,-0.512207763929782,
94.9978423713254));
#10226=CARTESIAN_POINT('Ctrl Pts',(1.87855338009975,-0.68654299343533,94.9858461317687));
#10227=CARTESIAN_POINT('Ctrl Pts',(1.82334749995286,-0.822006467192766,
94.9757031394992));
#10228=CARTESIAN_POINT('Ctrl Pts',(1.71177446885238,-1.0279448039999,94.9593612284853));
#10229=CARTESIAN_POINT('Ctrl Pts',(1.66453984848377,-1.10279278426571,94.9532115513421));
#10230=CARTESIAN_POINT('Ctrl Pts',(1.59766696571887,-1.19462212411728,94.9455864470728));
#10231=CARTESIAN_POINT('Ctrl Pts',(1.58245720008408,-1.21469794714771,94.9439144924345));
#10232=CARTESIAN_POINT('Ctrl Pts',(1.55791419072324,-1.24584926073553,94.9413190890251));
#10233=CARTESIAN_POINT('Ctrl Pts',(1.54883408112337,-1.25711973448196,94.9403798573355));
#10234=CARTESIAN_POINT('Ctrl Pts',(1.5306563100003,-1.27918649865755,94.9385421608716));
#10235=CARTESIAN_POINT('Ctrl Pts',(1.52156519604381,-1.28998690452822,94.9376433913933));
#10236=CARTESIAN_POINT('Ctrl Pts',(1.49708626919025,-1.31844944579232,94.9352738577021));
#10237=CARTESIAN_POINT('Ctrl Pts',(1.48150018175619,-1.33593920619831,94.9338167763371));
#10238=CARTESIAN_POINT('Ctrl Pts',(1.38381720636386,-1.44174041191605,94.92496617921));
#10239=CARTESIAN_POINT('Ctrl Pts',(1.29415178834417,-1.52274210553938,94.9180209318477));
#10240=CARTESIAN_POINT('Ctrl Pts',(1.11212782056348,-1.6594133209955,94.9048220050446));
#10241=CARTESIAN_POINT('Ctrl Pts',(1.02152152690275,-1.71667466565261,94.8985988335062));
#10242=CARTESIAN_POINT('Ctrl Pts',(0.891124553348857,-1.78508947791917,
94.8896944792892));
#10243=CARTESIAN_POINT('Ctrl Pts',(0.854928997228063,-1.80270449208195,
94.8872294129879));
#10244=CARTESIAN_POINT('Ctrl Pts',(0.795417981461111,-1.82947077154647,
94.8831713582245));
#10245=CARTESIAN_POINT('Ctrl Pts',(0.772418700767902,-1.83929941253145,
94.8816019034032));
#10246=CARTESIAN_POINT('Ctrl Pts',(0.72728685582231,-1.85759052815895,94.8785167332748));
#10247=CARTESIAN_POINT('Ctrl Pts',(0.705176261857091,-1.86609621950026,
94.8770028063069));
#10248=CARTESIAN_POINT('Ctrl Pts',(0.650853481422376,-1.88589026949441,
94.873274938858));
#10249=CARTESIAN_POINT('Ctrl Pts',(0.618493943138326,-1.89674915734738,
94.8710471496236));
#10250=CARTESIAN_POINT('Ctrl Pts',(0.437347017908791,-1.95240822628186,
94.8585293213655));
#10251=CARTESIAN_POINT('Ctrl Pts',(0.28401948116203,-1.98052696612134,94.8477003508948));
#10252=CARTESIAN_POINT('Ctrl Pts',(0.0463333531054047,-1.99593240325661,
94.8310914956814));
#10253=CARTESIAN_POINT('Ctrl Pts',(-0.0366113899861371,-1.9961349651935,
94.8253419842448));
#10254=CARTESIAN_POINT('Ctrl Pts',(-0.143851229570361,-1.98970792664064,
94.81813780822));
#10255=CARTESIAN_POINT('Ctrl Pts',(-0.168340459620043,-1.98778581095932,
94.8165085430132));
#10256=CARTESIAN_POINT('Ctrl Pts',(-0.207068256653312,-1.98402522990132,
94.8139635693902));
#10257=CARTESIAN_POINT('Ctrl Pts',(-0.221332457634056,-1.98248464050104,
94.81303302242));
#10258=CARTESIAN_POINT('Ctrl Pts',(-0.247983695250929,-1.97931495582176,
94.8113087157904));
#10259=CARTESIAN_POINT('Ctrl Pts',(-0.260374301620065,-1.97772314767735,
94.8105128894812));
#10260=CARTESIAN_POINT('Ctrl Pts',(-0.29461631657724,-1.97299671976163,
94.8083277114931));
#10261=CARTESIAN_POINT('Ctrl Pts',(-0.316432610203252,-1.96961552833803,
94.8069514447082));
#10262=CARTESIAN_POINT('Ctrl Pts',(-0.469086759411744,-1.94335441541403,
94.7974051694603));
#10263=CARTESIAN_POINT('Ctrl Pts',(-0.597424957286881,-1.90781582519287,
94.7897972057455));
#10264=CARTESIAN_POINT('Ctrl Pts',(-0.818379850211406,-1.82212139989698,
94.7760437422254));
#10265=CARTESIAN_POINT('Ctrl Pts',(-0.912363128409627,-1.77692503036384,
94.7699604989349));
#10266=CARTESIAN_POINT('Ctrl Pts',(-1.03425322739517,-1.70607929316196,
94.7613974419449));
#10267=CARTESIAN_POINT('Ctrl Pts',(-1.06560088140683,-1.6866774406634,94.7591313624949));
#10268=CARTESIAN_POINT('Ctrl Pts',(-1.11676936485749,-1.65301202469281,
94.7553128672792));
#10269=CARTESIAN_POINT('Ctrl Pts',(-1.13689871103542,-1.63923268756043,
94.7537786531774));
#10270=CARTESIAN_POINT('Ctrl Pts',(-1.17668338959991,-1.61091317322565,
94.7506784710887));
#10271=CARTESIAN_POINT('Ctrl Pts',(-1.19633413918716,-1.59637388794437,
94.749112711366));
#10272=CARTESIAN_POINT('Ctrl Pts',(-1.24516197761499,-1.55883899763492,
94.7451315420696));
#10273=CARTESIAN_POINT('Ctrl Pts',(-1.27397201865552,-1.53538345699506,
94.7426981853701));
#10274=CARTESIAN_POINT('Ctrl Pts',(-1.39792537087027,-1.42857606464283,
94.731842998691));
#10275=CARTESIAN_POINT('Ctrl Pts',(-1.4856585814445,-1.33709933737728,94.7230942628763));
#10276=CARTESIAN_POINT('Ctrl Pts',(-1.61122987556561,-1.17844192674678,
94.7089757223603));
#10277=CARTESIAN_POINT('Ctrl Pts',(-1.65489577017786,-1.11629204553124,
94.7036712708942));
#10278=CARTESIAN_POINT('Ctrl Pts',(-1.71101225266918,-1.02586382855634,
94.696382108899));
#10279=CARTESIAN_POINT('Ctrl Pts',(-1.72651249531619,-0.999557059447308,
94.6943096803854));
#10280=CARTESIAN_POINT('Ctrl Pts',(-1.75304784994849,-0.952061336780932,
94.6906654158869));
#10281=CARTESIAN_POINT('Ctrl Pts',(-1.76431771260774,-0.931010571136016,
94.6890832373839));
#10282=CARTESIAN_POINT('Ctrl Pts',(-1.78168680844721,-0.897118446140278,
94.6865939734653));
#10283=CARTESIAN_POINT('Ctrl Pts',(-1.78803114405685,-0.88440604439966,
94.685673063538));
#10284=CARTESIAN_POINT('Ctrl Pts',(-1.80051842169671,-0.858701035039137,
94.6838381313032));
#10285=CARTESIAN_POINT('Ctrl Pts',(-1.80665784649302,-0.845707698218548,
94.6829243335641));
#10286=CARTESIAN_POINT('Ctrl Pts',(-1.82295750055046,-0.810223735175114,
94.6804628630978));
#10287=CARTESIAN_POINT('Ctrl Pts',(-1.83284198127424,-0.787608374228948,
94.6789308326135));
#10288=CARTESIAN_POINT('Ctrl Pts',(-1.8741878208184,-0.688013422227519,
94.6723186152871));
#10289=CARTESIAN_POINT('Ctrl Pts',(-1.9012405036474,-0.60928621840954,94.6674368873436));
#10290=CARTESIAN_POINT('Ctrl Pts',(-1.94315050863123,-0.456939609295913,
94.6582433561534));
#10291=CARTESIAN_POINT('Ctrl Pts',(-1.95892355149556,-0.383726693627432,
94.6539306291679));
#10292=CARTESIAN_POINT('Ctrl Pts',(-1.97965101114832,-0.251885878741675,
94.6461314979659));
#10293=CARTESIAN_POINT('Ctrl Pts',(-1.98619806998029,-0.193600586003824,
94.6426728484757));
#10294=CARTESIAN_POINT('Ctrl Pts',(-1.99321318099655,-0.0902714636182581,
94.6364442687785));
#10295=CARTESIAN_POINT('Ctrl Pts',(-1.99474094538159,-0.0453412368257697,
94.6337039991689));
#10296=CARTESIAN_POINT('Ctrl Pts',(-1.99475515014938,0.0254756584597319,
94.6293124195342));
#10297=CARTESIAN_POINT('Ctrl Pts',(-1.99425685285608,0.0513480592313933,
94.6276928372794));
#10298=CARTESIAN_POINT('Ctrl Pts',(-1.9923424517438,0.100775079815879,94.6245661517782));
#10299=CARTESIAN_POINT('Ctrl Pts',(-1.99101139003775,0.124328707273745,
94.6230619980674));
#10300=CARTESIAN_POINT('Ctrl Pts',(-1.98690200403548,0.179617971685833,
94.619495442874));
#10301=CARTESIAN_POINT('Ctrl Pts',(-1.98378060979329,0.211320813876593,
94.6174225667285));
#10302=CARTESIAN_POINT('Ctrl Pts',(-1.9688021423382,0.333394744469055,94.6093282535835));
#10303=CARTESIAN_POINT('Ctrl Pts',(-1.95151755653796,0.422976674579823,
94.6031422473714));
#10304=CARTESIAN_POINT('Ctrl Pts',(-1.91010256459144,0.57923288766905,94.5919691421925));
#10305=CARTESIAN_POINT('Ctrl Pts',(-1.88842884801342,0.646404293885178,
94.5870365336252));
#10306=CARTESIAN_POINT('Ctrl Pts',(-1.83407770900289,0.788579857640487,
94.5764240467774));
#10307=CARTESIAN_POINT('Ctrl Pts',(-1.80025018444409,0.863018362847558,
94.5707583942592));
#10308=CARTESIAN_POINT('Ctrl Pts',(-1.75039987305223,0.956940369494432,
94.5636271569895));
#10309=CARTESIAN_POINT('Ctrl Pts',(-1.73844631861725,0.97848817864638,94.561992624652));
#10310=CARTESIAN_POINT('Ctrl Pts',(-1.71889756798875,1.01223760692697,94.5594414265673));
#10311=CARTESIAN_POINT('Ctrl Pts',(-1.71156488974823,1.02458746879418,94.5585098067686));
#10312=CARTESIAN_POINT('Ctrl Pts',(-1.69671073008836,1.04900062224592,94.5566737249281));
#10313=CARTESIAN_POINT('Ctrl Pts',(-1.68919244049364,1.06106481073259,94.5557691690028));
#10314=CARTESIAN_POINT('Ctrl Pts',(-1.67675295115384,1.08055841072364,94.5543103505775));
#10315=CARTESIAN_POINT('Ctrl Pts',(-1.67191004952877,1.08803663755448,94.5537513883947));
#10316=CARTESIAN_POINT('Ctrl Pts',(-1.66701720848889,1.09548217196899,94.5531952825684));
#10317=CARTESIAN_POINT('Ctrl Pts',(-1.66701746607045,1.09548178000186,94.3957559446131));
#10318=CARTESIAN_POINT('Ctrl Pts',(-1.72234085055941,1.0112950322998,94.4026072520028));
#10319=CARTESIAN_POINT('Ctrl Pts',(-1.77123728885008,0.922992974446591,
94.4096419874811));
#10320=CARTESIAN_POINT('Ctrl Pts',(-1.84990319857548,0.751408149615364,
94.4228114350097));
#10321=CARTESIAN_POINT('Ctrl Pts',(-1.88122093678841,0.66915342018724,94.4289257276447));
#10322=CARTESIAN_POINT('Ctrl Pts',(-1.91438130181607,0.561073221213647,
94.4365135640341));
#10323=CARTESIAN_POINT('Ctrl Pts',(-1.92129735696453,0.536912966604122,
94.438181669056));
#10324=CARTESIAN_POINT('Ctrl Pts',(-1.93147103579295,0.498654433812127,
94.4407723694985));
#10325=CARTESIAN_POINT('Ctrl Pts',(-1.93503477698584,0.48464115568311,94.4417106638947));
#10326=CARTESIAN_POINT('Ctrl Pts',(-1.94177710867641,0.456868253884788,
94.4435476402762));
#10327=CARTESIAN_POINT('Ctrl Pts',(-1.94496255449358,0.443111301035664,
94.4444466090214));
#10328=CARTESIAN_POINT('Ctrl Pts',(-1.95304993685363,0.406415625350268,
94.4468182731131));
#10329=CARTESIAN_POINT('Ctrl Pts',(-1.95769399326869,0.383421515032688,
94.4482772346208));
#10330=CARTESIAN_POINT('Ctrl Pts',(-1.98365164534925,0.242094518024507,
94.4571082998858));
#10331=CARTESIAN_POINT('Ctrl Pts',(-1.9946381206811,0.122103299536532,94.464035045935));
#10332=CARTESIAN_POINT('Ctrl Pts',(-1.99485382532739,-0.111537975921789,
94.4775828400643));
#10333=CARTESIAN_POINT('Ctrl Pts',(-1.9852921665754,-0.224709168571586,
94.4841770799989));
#10334=CARTESIAN_POINT('Ctrl Pts',(-1.95989974512443,-0.373099245030639,
94.49331692478));
#10335=CARTESIAN_POINT('Ctrl Pts',(-1.95260521739944,-0.409563976140234,
94.4956018757191));
#10336=CARTESIAN_POINT('Ctrl Pts',(-1.93883316378939,-0.469628670061659,
94.4994426540661));
#10337=CARTESIAN_POINT('Ctrl Pts',(-1.93293267397357,-0.493352122937258,
94.5009797886316));
#10338=CARTESIAN_POINT('Ctrl Pts',(-1.92028032840084,-0.540504643114598,
94.5040783918586));
#10339=CARTESIAN_POINT('Ctrl Pts',(-1.91353191742561,-0.563930245920264,
94.5056395149832));
#10340=CARTESIAN_POINT('Ctrl Pts',(-1.89552229117753,-0.622396310368928,
94.5095930982492));
#10341=CARTESIAN_POINT('Ctrl Pts',(-1.88371783338206,-0.657258510208223,
94.512002996197));
#10342=CARTESIAN_POINT('Ctrl Pts',(-1.83498734577181,-0.789054196339219,
94.5213208978034));
#10343=CARTESIAN_POINT('Ctrl Pts',(-1.79149044277126,-0.883369610399564,
94.5284358580718));
#10344=CARTESIAN_POINT('Ctrl Pts',(-1.67567408528248,-1.09040106452989,
94.5449391366079));
#10345=CARTESIAN_POINT('Ctrl Pts',(-1.5989425966499,-1.20010198722774,94.5543599074582));
#10346=CARTESIAN_POINT('Ctrl Pts',(-1.49747402565541,-1.31798434826651,
94.5647442706119));
#10347=CARTESIAN_POINT('Ctrl Pts',(-1.48285185569662,-1.33441435510216,
94.5661975063757));
#10348=CARTESIAN_POINT('Ctrl Pts',(-1.45951349449258,-1.35978070111148,
94.568445970764));
#10349=CARTESIAN_POINT('Ctrl Pts',(-1.45098049411716,-1.36888232677686,
94.5692537347906));
#10350=CARTESIAN_POINT('Ctrl Pts',(-1.43244180215702,-1.38828826393017,
94.5709769893516));
#10351=CARTESIAN_POINT('Ctrl Pts',(-1.42240902672103,-1.39856584101785,
94.5718902871724));
#10352=CARTESIAN_POINT('Ctrl Pts',(-1.39485738025176,-1.42618654997126,
94.5743495602532));
#10353=CARTESIAN_POINT('Ctrl Pts',(-1.37712607675265,-1.44331531015171,
94.5758799348214));
#10354=CARTESIAN_POINT('Ctrl Pts',(-1.29784945597035,-1.51710646432063,
94.582521202334));
#10355=CARTESIAN_POINT('Ctrl Pts',(-1.23308714688521,-1.57019873161565,
94.5874309014939));
#10356=CARTESIAN_POINT('Ctrl Pts',(-1.04021287089503,-1.70900209521139,
94.6012556493916));
#10357=CARTESIAN_POINT('Ctrl Pts',(-0.905270696982442,-1.78415584065899,
94.6100631946339));
#10358=CARTESIAN_POINT('Ctrl Pts',(-0.731321434214433,-1.85617198949191,
94.6215405815396));
#10359=CARTESIAN_POINT('Ctrl Pts',(-0.69927868039424,-1.86847922213847,
94.6236570949731));
#10360=CARTESIAN_POINT('Ctrl Pts',(-0.64458601544131,-1.88788209684428,
94.6272828391324));
#10361=CARTESIAN_POINT('Ctrl Pts',(-0.622097422547269,-1.89541147545236,
94.628777316197));
#10362=CARTESIAN_POINT('Ctrl Pts',(-0.575687301915362,-1.91003508518783,
94.6318715994443));
#10363=CARTESIAN_POINT('Ctrl Pts',(-0.551756304930712,-1.9170849699942,
94.6334725642319));
#10364=CARTESIAN_POINT('Ctrl Pts',(-0.489192642572395,-1.93424728039212,
94.6376746892442));
#10365=CARTESIAN_POINT('Ctrl Pts',(-0.450379009383618,-1.94365129394204,
94.6402981394614));
#10366=CARTESIAN_POINT('Ctrl Pts',(-0.298048564977516,-1.97575119060712,
94.6506635346371));
#10367=CARTESIAN_POINT('Ctrl Pts',(-0.182937796229097,-1.9897117387946,
94.658661872608));
#10368=CARTESIAN_POINT('Ctrl Pts',(0.0440314465671003,-1.9973716754297,
94.6745026431037));
#10369=CARTESIAN_POINT('Ctrl Pts',(0.155471852321721,-1.99179929765975,
94.682308631613));
#10370=CARTESIAN_POINT('Ctrl Pts',(0.289658813082551,-1.97375313436064,
94.6913797609719));
#10371=CARTESIAN_POINT('Ctrl Pts',(0.313388380668226,-1.97012474462161,
94.6929706944434));
#10372=CARTESIAN_POINT('Ctrl Pts',(0.351073161289664,-1.96366435191211,
94.6954701488235));
#10373=CARTESIAN_POINT('Ctrl Pts',(0.365072862796352,-1.96110986152983,
94.6963926829507));
#10374=CARTESIAN_POINT('Ctrl Pts',(0.393119375069116,-1.95568152830216,
94.6982271523147));
#10375=CARTESIAN_POINT('Ctrl Pts',(0.407164912396803,-1.95280563492537,
94.6991389232492));
#10376=CARTESIAN_POINT('Ctrl Pts',(0.445149487690522,-1.94460044857614,
94.70158891864));
#10377=CARTESIAN_POINT('Ctrl Pts',(0.469023988048549,-1.93898055613956,
94.7031117428312));
#10378=CARTESIAN_POINT('Ctrl Pts',(0.572789215257659,-1.91252605846039,
94.7096797066495));
#10379=CARTESIAN_POINT('Ctrl Pts',(0.651453257493272,-1.88718168619305,
94.7145287383811));
#10380=CARTESIAN_POINT('Ctrl Pts',(0.873467432677757,-1.80010789860049,
94.7284076062172));
#10381=CARTESIAN_POINT('Ctrl Pts',(1.0114211788061,-1.72637109465251,94.7373199644767));
#10382=CARTESIAN_POINT('Ctrl Pts',(1.16732780025472,-1.61787905999709,94.748904218046));
#10383=CARTESIAN_POINT('Ctrl Pts',(1.19477131620079,-1.59771966704374,94.7510046580032));
#10384=CARTESIAN_POINT('Ctrl Pts',(1.24039657803675,-1.56237134365112,94.754611567818));
#10385=CARTESIAN_POINT('Ctrl Pts',(1.2588486276319,-1.54754254897465,94.7561036703488));
#10386=CARTESIAN_POINT('Ctrl Pts',(1.29625432672046,-1.51637014120827,94.7592007090007));
#10387=CARTESIAN_POINT('Ctrl Pts',(1.31517294847959,-1.49999123509994,94.7608069420687));
#10388=CARTESIAN_POINT('Ctrl Pts',(1.3637743533284,-1.45628789726547,94.7650417173248));
#10389=CARTESIAN_POINT('Ctrl Pts',(1.39294382588228,-1.42841241744161,94.7676932150616));
#10390=CARTESIAN_POINT('Ctrl Pts',(1.50100631575798,-1.31868436363296,94.7779525906848));
#10391=CARTESIAN_POINT('Ctrl Pts',(1.57368729988192,-1.231036302203,94.7858046002336));
#10392=CARTESIAN_POINT('Ctrl Pts',(1.70283212427025,-1.04504177996186,94.8015971935676));
#10393=CARTESIAN_POINT('Ctrl Pts',(1.75919253802137,-0.947098086779131,
94.809505951235));
#10394=CARTESIAN_POINT('Ctrl Pts',(1.8171125464336,-0.823226867615654,94.8186664337049));
#10395=CARTESIAN_POINT('Ctrl Pts',(1.82686038939481,-0.80136241604765,94.8202528170724));
#10396=CARTESIAN_POINT('Ctrl Pts',(1.84176701244387,-0.766240132792765,
94.8227468897498));
#10397=CARTESIAN_POINT('Ctrl Pts',(1.84718138185248,-0.753094047832167,
94.8236684952487));
#10398=CARTESIAN_POINT('Ctrl Pts',(1.85777771673606,-0.7265641374833,94.8255029093264));
#10399=CARTESIAN_POINT('Ctrl Pts',(1.86295671400261,-0.713180063514287,
94.8264155245002));
#10400=CARTESIAN_POINT('Ctrl Pts',(1.87661821622744,-0.676710038575338,
94.8288706521999));
#10401=CARTESIAN_POINT('Ctrl Pts',(1.88481922127824,-0.653520494951424,
94.8303976536703));
#10402=CARTESIAN_POINT('Ctrl Pts',(1.91886223526572,-0.551281377037774,
94.8370060744766));
#10403=CARTESIAN_POINT('Ctrl Pts',(1.94017753753412,-0.4708049017683,94.8418885866826));
#10404=CARTESIAN_POINT('Ctrl Pts',(1.98661843337307,-0.23737400045742,94.8557373631577));
#10405=CARTESIAN_POINT('Ctrl Pts',(1.99904556621664,-0.0825358998770869,
94.8645917287909));
#10406=CARTESIAN_POINT('Ctrl Pts',(1.99220624355518,0.106355378428988,94.8761168360027));
#10407=CARTESIAN_POINT('Ctrl Pts',(1.99009008337187,0.140493513254606,94.8782262017423));
#10408=CARTESIAN_POINT('Ctrl Pts',(1.98502402816594,0.198163141345853,94.8818435629053));
#10409=CARTESIAN_POINT('Ctrl Pts',(1.98253014310789,0.221727707678418,94.883336976731));
#10410=CARTESIAN_POINT('Ctrl Pts',(1.9765460726311,0.270031809412018,94.8864324457461));
#10411=CARTESIAN_POINT('Ctrl Pts',(1.97300969222284,0.294761285302761,94.8880357205874));
#10412=CARTESIAN_POINT('Ctrl Pts',(1.96258719464009,0.359009607645426,94.8922521687871));
#10413=CARTESIAN_POINT('Ctrl Pts',(1.9549720846786,0.398396987146023,94.8948879233356));
#10414=CARTESIAN_POINT('Ctrl Pts',(1.92244444056224,0.543084443519314,94.9047643240906));
#10415=CARTESIAN_POINT('Ctrl Pts',(1.89016782667402,0.646524069356427,94.9122226308457));
#10416=CARTESIAN_POINT('Ctrl Pts',(1.80494395005695,0.857599197321721,94.928088048193));
#10417=CARTESIAN_POINT('Ctrl Pts',(1.75035397216493,0.964138895694782,94.9364821087725));
#10418=CARTESIAN_POINT('Ctrl Pts',(1.67398858491842,1.08505462977537,94.9460560530447));
#10419=CARTESIAN_POINT('Ctrl Pts',(1.66107100996395,1.10472826914306,94.9476147835699));
#10420=CARTESIAN_POINT('Ctrl Pts',(1.63984152028889,1.13584644927539,94.950076173487));
#10421=CARTESIAN_POINT('Ctrl Pts',(1.63175114562176,1.14743871419964,94.9509921626206));
#10422=CARTESIAN_POINT('Ctrl Pts',(1.61514803684204,1.17069761510358,94.9528265059667));
#10423=CARTESIAN_POINT('Ctrl Pts',(1.60663052750775,1.18235970248587,94.9537444850996));
#10424=CARTESIAN_POINT('Ctrl Pts',(1.58300058105899,1.21398666885885,94.9562322375093));
#10425=CARTESIAN_POINT('Ctrl Pts',(1.5676372191505,1.23376179049795,94.9577857885204));
#10426=CARTESIAN_POINT('Ctrl Pts',(1.49718196231678,1.32100729039596,94.964657468642));
#10427=CARTESIAN_POINT('Ctrl Pts',(1.43807383832485,1.3851211928176,94.9697579947416));
#10428=CARTESIAN_POINT('Ctrl Pts',(1.26772136879738,1.54719722538085,94.9834249292052));
#10429=CARTESIAN_POINT('Ctrl Pts',(1.14947278465562,1.63696215773694,94.9919113685094));
#10430=CARTESIAN_POINT('Ctrl Pts',(0.992228677138516,1.73082159466148,95.0030618471947));
#10431=CARTESIAN_POINT('Ctrl Pts',(0.961601768133306,1.74802258200071,95.0052255674762));
#10432=CARTESIAN_POINT('Ctrl Pts',(0.909446087625864,1.77552921420515,95.008906900898));
#10433=CARTESIAN_POINT('Ctrl Pts',(0.888157049798099,1.78627353785805,95.0104086110769));
#10434=CARTESIAN_POINT('Ctrl Pts',(0.844395305354261,1.80738384643756,95.0134963594836));
#10435=CARTESIAN_POINT('Ctrl Pts',(0.82191214831249,1.81771838545395,95.0150831696287));
#10436=CARTESIAN_POINT('Ctrl Pts',(0.763670283496213,1.84318819218763,95.0191974678284));
#10437=CARTESIAN_POINT('Ctrl Pts',(0.727652804076258,1.85770182253066,95.0217454889645));
#10438=CARTESIAN_POINT('Ctrl Pts',(0.646634499047044,1.8876313827665,95.0274882628434));
#10439=CARTESIAN_POINT('Ctrl Pts',(0.601460371254185,1.9025071017558,95.0306979817946));
#10440=CARTESIAN_POINT('Ctrl Pts',(0.438258094034412,1.94985552764731,95.0423076705302));
#10441=CARTESIAN_POINT('Ctrl Pts',(0.31783104822713,1.97306522650949,95.0509192155384));
#10442=CARTESIAN_POINT('Ctrl Pts',(0.184560515937871,1.9862271427577,95.0602094352488));
#10443=CARTESIAN_POINT('Ctrl Pts',(0.173061783772749,1.98726205392293,95.061008880912));
#10444=CARTESIAN_POINT('Ctrl Pts',(0.104965202839168,1.99279536662306,95.0657287028701));
#10445=CARTESIAN_POINT('Ctrl Pts',(0.0482001199276148,1.99497592331722,
95.0696043153805));
#10446=CARTESIAN_POINT('Ctrl Pts',(-0.0281025192915678,1.99464752442088,
95.0746734183335));
#10447=CARTESIAN_POINT('Ctrl Pts',(-0.0476185473319972,1.99427707268691,
95.0759575354909));
#10448=CARTESIAN_POINT('Ctrl Pts',(-0.0805583133211505,1.99316796301811,
95.0781004659385));
#10449=CARTESIAN_POINT('Ctrl Pts',(-0.0939852496088416,1.99257998218247,
95.0789670061351));
#10450=CARTESIAN_POINT('Ctrl Pts',(-0.123255387817326,1.9910016559093,95.0808400429614));
#10451=CARTESIAN_POINT('Ctrl Pts',(-0.139094273582351,1.98995786570135,
95.0818436976671));
#10452=CARTESIAN_POINT('Ctrl Pts',(-0.187370481802562,1.98619719890168,
95.0848771788734));
#10453=CARTESIAN_POINT('Ctrl Pts',(-0.219756705741729,1.98287525378018,
95.0868768824646));
#10454=CARTESIAN_POINT('Ctrl Pts',(-0.298986281507957,1.97278321373854,
95.0917137533449));
#10455=CARTESIAN_POINT('Ctrl Pts',(-0.345698646081356,1.96513596588499,
95.0945179806292));
#10456=CARTESIAN_POINT('Ctrl Pts',(-0.550676055505781,1.92404297133538,
95.1067796885204));
#10457=CARTESIAN_POINT('Ctrl Pts',(-0.704792316380372,1.87308655043888,
95.1159372905321));
#10458=CARTESIAN_POINT('Ctrl Pts',(-0.889040091783791,1.78616856279797,
95.1282301844786));
#10459=CARTESIAN_POINT('Ctrl Pts',(-0.926435920998179,1.76706155101298,
95.1307972231268));
#10460=CARTESIAN_POINT('Ctrl Pts',(-0.9853778621583,1.73456031524067,95.1349784261133));
#10461=CARTESIAN_POINT('Ctrl Pts',(-1.00732074902634,1.72190993750723,95.1365661299273));
#10462=CARTESIAN_POINT('Ctrl Pts',(-1.04939238985302,1.69657564603989,95.1396746518579));
#10463=CARTESIAN_POINT('Ctrl Pts',(-1.06954685533006,1.68394262186445,95.1411934068288));
#10464=CARTESIAN_POINT('Ctrl Pts',(-1.11733484843794,1.65278459955141,95.1448687162549));
#10465=CARTESIAN_POINT('Ctrl Pts',(-1.14473946256447,1.63392332654914,95.1470376584428));
#10466=CARTESIAN_POINT('Ctrl Pts',(-1.26955969096458,1.54333370795849,95.1572116389215));
#10467=CARTESIAN_POINT('Ctrl Pts',(-1.36077988903793,1.46353355744171,95.1655256470115));
#10468=CARTESIAN_POINT('Ctrl Pts',(-1.5267316245529,1.28935386566257,95.182289761695));
#10469=CARTESIAN_POINT('Ctrl Pts',(-1.60130511782977,1.19547757932092,95.1907000296954));
#10470=CARTESIAN_POINT('Ctrl Pts',(-1.66701720893993,1.09548217128264,95.1987207124569));
#10471=CARTESIAN_POINT('Origin',(0.,0.,89.2710285354474));
#10472=CARTESIAN_POINT('',(-1.66701720827332,1.09548217229703,96.1569262941178));
#10473=CARTESIAN_POINT('',(-1.66701720851842,1.09548217192407,95.9972028497351));
#10474=CARTESIAN_POINT('',(-1.66701720851066,1.09548217193587,89.2710285354474));
#10475=CARTESIAN_POINT('',(-1.99474928355678,-0.00169063588936904,95.428322530593));
#10476=CARTESIAN_POINT('Ctrl Pts',(-1.66701720827332,1.09548217229703,96.1569262941178));
#10477=CARTESIAN_POINT('Ctrl Pts',(-1.65718555120821,1.11044320217762,96.155810481867));
#10478=CARTESIAN_POINT('Ctrl Pts',(-1.64715299206609,1.12527110996234,96.1546873293238));
#10479=CARTESIAN_POINT('Ctrl Pts',(-1.62356010618087,1.15914918914147,96.1520796164126));
#10480=CARTESIAN_POINT('Ctrl Pts',(-1.60986214623897,1.17809933957545,96.1505898928457));
#10481=CARTESIAN_POINT('Ctrl Pts',(-1.57753446881027,1.22120551531339,96.1471263981644));
#10482=CARTESIAN_POINT('Ctrl Pts',(-1.55867783592543,1.24518317611485,96.1451438338539));
#10483=CARTESIAN_POINT('Ctrl Pts',(-1.4921193017721,1.32593571544113,96.1382672384479));
#10484=CARTESIAN_POINT('Ctrl Pts',(-1.44181061195347,1.38047292060104,96.1332697996111));
#10485=CARTESIAN_POINT('Ctrl Pts',(-1.38203403040671,1.43843416697403,96.1275555004801));
#10486=CARTESIAN_POINT('Ctrl Pts',(-1.37543610621948,1.44474441636437,96.1269276819358));
#10487=CARTESIAN_POINT('Ctrl Pts',(-1.28157730318415,1.53328519495493,96.1180383372285));
#10488=CARTESIAN_POINT('Ctrl Pts',(-1.1871238639983,1.60752573190601,96.1095775453159));
#10489=CARTESIAN_POINT('Ctrl Pts',(-1.04037214602199,1.70284738486894,96.0974967694941));
#10490=CARTESIAN_POINT('Ctrl Pts',(-0.992937490984979,1.73093605376192,
96.0937401661729));
#10491=CARTESIAN_POINT('Ctrl Pts',(-0.927753039315384,1.76597250905472,
96.0888288798244));
#10492=CARTESIAN_POINT('Ctrl Pts',(-0.910982307948996,1.77468191635101,
96.0875868367289));
#10493=CARTESIAN_POINT('Ctrl Pts',(-0.882177375235394,1.78912498667104,
96.0854932014088));
#10494=CARTESIAN_POINT('Ctrl Pts',(-0.870205448786078,1.79497845475207,
96.0846346607371));
#10495=CARTESIAN_POINT('Ctrl Pts',(-0.843600057448697,1.80765792400793,
96.0827527240333));
#10496=CARTESIAN_POINT('Ctrl Pts',(-0.828941076879176,1.81442689569141,
96.0817326583937));
#10497=CARTESIAN_POINT('Ctrl Pts',(-0.783067525646691,1.83493756667492,
96.078587656144));
#10498=CARTESIAN_POINT('Ctrl Pts',(-0.751580153335586,1.84805795459866,
96.0764961673729));
#10499=CARTESIAN_POINT('Ctrl Pts',(-0.672463065625395,1.87866812138816,
96.0713694873987));
#10500=CARTESIAN_POINT('Ctrl Pts',(-0.624472549307504,1.89516097391315,
96.0683726624658));
#10501=CARTESIAN_POINT('Ctrl Pts',(-0.410838420465918,1.95958240964507,
96.0553176215227));
#10502=CARTESIAN_POINT('Ctrl Pts',(-0.240030758218407,1.98774617780153,
96.045548388951));
#10503=CARTESIAN_POINT('Ctrl Pts',(-0.0337182590463221,1.99475530458375,
96.0329572928333));
#10504=CARTESIAN_POINT('Ctrl Pts',(0.000315049989103523,1.99504018350141,
96.0308577792975));
#10505=CARTESIAN_POINT('Ctrl Pts',(0.0580354930702617,1.99404644006744,
96.0272498697896));
#10506=CARTESIAN_POINT('Ctrl Pts',(0.0817234549550927,1.99321612531343,
96.0257557667319));
#10507=CARTESIAN_POINT('Ctrl Pts',(0.130450312191673,1.99063810011081,96.022651994938));
#10508=CARTESIAN_POINT('Ctrl Pts',(0.155482164603916,1.98883949339408,96.0210409808045));
#10509=CARTESIAN_POINT('Ctrl Pts',(0.220879619033977,1.98289837510018,96.0167860760089));
#10510=CARTESIAN_POINT('Ctrl Pts',(0.261162682853044,1.97799581126181,96.0141189298242));
#10511=CARTESIAN_POINT('Ctrl Pts',(0.404687675438619,1.95606778243425,96.0044453799975));
#10512=CARTESIAN_POINT('Ctrl Pts',(0.506693356665096,1.93215685501721,95.9972403429969));
#10513=CARTESIAN_POINT('Ctrl Pts',(0.722599765512278,1.86326836870318,95.9814565039718));
#10514=CARTESIAN_POINT('Ctrl Pts',(0.835215392179229,1.81558214297996,95.9728788030905));
#10515=CARTESIAN_POINT('Ctrl Pts',(0.9632559709393,1.74691321743989,95.9631589077026));
#10516=CARTESIAN_POINT('Ctrl Pts',(0.983547713442134,1.73556960758609,95.9616201818055));
#10517=CARTESIAN_POINT('Ctrl Pts',(1.01582550046536,1.7167775079078,95.9591807824589));
#10518=CARTESIAN_POINT('Ctrl Pts',(1.02793842142351,1.7095523093668,95.9582672578376));
#10519=CARTESIAN_POINT('Ctrl Pts',(1.05239437531223,1.69461071663575,95.9564283527891));
#10520=CARTESIAN_POINT('Ctrl Pts',(1.06473152646805,1.6868865434114,95.9555035117789));
#10521=CARTESIAN_POINT('Ctrl Pts',(1.09848804373676,1.66523400559506,95.9529776110545));
#10522=CARTESIAN_POINT('Ctrl Pts',(1.11972679971511,1.65102765322497,95.9513935735834));
#10523=CARTESIAN_POINT('Ctrl Pts',(1.16816686839282,1.61726179827986,95.9477784856478));
#10524=CARTESIAN_POINT('Ctrl Pts',(1.19516046813669,1.59741705369019,95.9457621795953));
#10525=CARTESIAN_POINT('Ctrl Pts',(1.2935353372021,1.52120494122501,95.9383561048706));
#10526=CARTESIAN_POINT('Ctrl Pts',(1.36153853727005,1.46065487294374,95.9331154899632));
#10527=CARTESIAN_POINT('Ctrl Pts',(1.49906087726493,1.32022552824929,95.9217098969715));
#10528=CARTESIAN_POINT('Ctrl Pts',(1.56683185762389,1.23903749061577,95.9155455065653));
#10529=CARTESIAN_POINT('Ctrl Pts',(1.64924950321509,1.12266373824548,95.9068854237849));
#10530=CARTESIAN_POINT('Ctrl Pts',(1.66979722993901,1.09186754478085,95.9046100654212));
#10531=CARTESIAN_POINT('Ctrl Pts',(1.70246339748899,1.03982822558492,95.9007798802223));
#10532=CARTESIAN_POINT('Ctrl Pts',(1.71506973619169,1.01890140506983,95.8992434705017));
#10533=CARTESIAN_POINT('Ctrl Pts',(1.73950888353016,0.976592721752463,95.8961418698856));
#10534=CARTESIAN_POINT('Ctrl Pts',(1.75133941670121,0.955214457279873,95.8945769432028));
#10535=CARTESIAN_POINT('Ctrl Pts',(1.78010632376555,0.900899770357549,95.8906041722798));
#10536=CARTESIAN_POINT('Ctrl Pts',(1.79652305659613,0.867700134478513,95.8881785693077));
#10537=CARTESIAN_POINT('Ctrl Pts',(1.85606519862452,0.738344823156949,95.8787326821863));
#10538=CARTESIAN_POINT('Ctrl Pts',(1.89246530539454,0.639297071433817,95.8714983211058));
#10539=CARTESIAN_POINT('Ctrl Pts',(1.95617953598975,0.411749413906618,95.8550521539249));
#10540=CARTESIAN_POINT('Ctrl Pts',(1.97898718761388,0.282470764603638,95.8458199947951));
#10541=CARTESIAN_POINT('Ctrl Pts',(1.99065701722765,0.129650966286144,95.8355816179709));
#10542=CARTESIAN_POINT('Ctrl Pts',(1.99198196647591,0.107390313759802,95.83410745844));
#10543=CARTESIAN_POINT('Ctrl Pts',(1.9934680891285,0.0725917276628886,95.8318346279011));
#10544=CARTESIAN_POINT('Ctrl Pts',(1.99388478295424,0.0600672482854625,
95.8310229961583));
#10545=CARTESIAN_POINT('Ctrl Pts',(1.99452376804397,0.0332630174499008,
95.8293008450244));
#10546=CARTESIAN_POINT('Ctrl Pts',(1.99471079723741,0.0189830075776515,
95.8283923890133));
#10547=CARTESIAN_POINT('Ctrl Pts',(1.99480164228288,-0.019558881247296,
95.8259618387166));
#10548=CARTESIAN_POINT('Ctrl Pts',(1.99441622854976,-0.0438197796222868,
95.8244547415938));
#10549=CARTESIAN_POINT('Ctrl Pts',(1.99084652767614,-0.148368527168874,
95.8180355355985));
#10550=CARTESIAN_POINT('Ctrl Pts',(1.98325540178347,-0.228437354466921,
95.8133095507038));
#10551=CARTESIAN_POINT('Ctrl Pts',(1.94617349370064,-0.465845780593805,
95.7993160740881));
#10552=CARTESIAN_POINT('Ctrl Pts',(1.90258484034827,-0.620298912835385,
95.7901882687197));
#10553=CARTESIAN_POINT('Ctrl Pts',(1.82814183536849,-0.798777248527106,
95.778383870874));
#10554=CARTESIAN_POINT('Ctrl Pts',(1.81448350939313,-0.829335308167921,
95.7763177076403));
#10555=CARTESIAN_POINT('Ctrl Pts',(1.78980391512241,-0.881020102060512,
95.7727364949512));
#10556=CARTESIAN_POINT('Ctrl Pts',(1.77916077291047,-0.902319976130327,
95.7712347582729));
#10557=CARTESIAN_POINT('Ctrl Pts',(1.75645196863676,-0.945802005943015,
95.7681126166698));
#10558=CARTESIAN_POINT('Ctrl Pts',(1.74434132155344,-0.967955685412192,
95.7664908081088));
#10559=CARTESIAN_POINT('Ctrl Pts',(1.71117845658708,-1.02597517580799,95.7621574830059));
#10560=CARTESIAN_POINT('Ctrl Pts',(1.68942049399444,-1.06142109442833,95.7594209284971));
#10561=CARTESIAN_POINT('Ctrl Pts',(1.61290398940453,-1.17775481282689,95.7501309443903));
#10562=CARTESIAN_POINT('Ctrl Pts',(1.55332227062096,-1.25528939990836,95.7434123740196));
#10563=CARTESIAN_POINT('Ctrl Pts',(1.40219170503602,-1.42464572957135,95.7276101657699));
#10564=CARTESIAN_POINT('Ctrl Pts',(1.30688670246067,-1.51255023759461,95.7184951895744));
#10565=CARTESIAN_POINT('Ctrl Pts',(1.18582176102637,-1.60416927630132,95.708349622307));
#10566=CARTESIAN_POINT('Ctrl Pts',(1.16767811949116,-1.61742394823665,95.7068638345312));
#10567=CARTESIAN_POINT('Ctrl Pts',(1.1390529759052,-1.63760296665094,95.7045779821658));
#10568=CARTESIAN_POINT('Ctrl Pts',(1.12872404715159,-1.64473925122031,95.7037647002753));
#10569=CARTESIAN_POINT('Ctrl Pts',(1.10653584936109,-1.65976166244187,95.7020432894067));
#10570=CARTESIAN_POINT('Ctrl Pts',(1.09465802692806,-1.66761931947711,95.7011371574348));
#10571=CARTESIAN_POINT('Ctrl Pts',(1.06250457039156,-1.68839853153055,95.6987223567505));
#10572=CARTESIAN_POINT('Ctrl Pts',(1.04207716071228,-1.70108226589601,95.6972283281254));
#10573=CARTESIAN_POINT('Ctrl Pts',(0.932835099552581,-1.7662059267947,95.6894207061942));
#10574=CARTESIAN_POINT('Ctrl Pts',(0.840273193861112,-1.81207348534812,
95.6834267565779));
#10575=CARTESIAN_POINT('Ctrl Pts',(0.624109702688555,-1.89904563305184,
95.6699117573346));
#10576=CARTESIAN_POINT('Ctrl Pts',(0.499216766717564,-1.93563067270597,
95.662414772899));
#10577=CARTESIAN_POINT('Ctrl Pts',(0.335327690412879,-1.9667105531926,95.6522846342544));
#10578=CARTESIAN_POINT('Ctrl Pts',(0.298812915084599,-1.97258856171814,
95.6500115522083));
#10579=CARTESIAN_POINT('Ctrl Pts',(0.237951651615745,-1.98065716329069,
95.6461844374645));
#10580=CARTESIAN_POINT('Ctrl Pts',(0.213689767485512,-1.98342138364617,
95.6446487788926));
#10581=CARTESIAN_POINT('Ctrl Pts',(0.165065138562273,-1.98805881538828,
95.6415481479632));
#10582=CARTESIAN_POINT('Ctrl Pts',(0.140706578795773,-1.98993113547655,
95.6399834294939));
#10583=CARTESIAN_POINT('Ctrl Pts',(0.0793384714745956,-1.99351581817488,
95.6360100296403));
#10584=CARTESIAN_POINT('Ctrl Pts',(0.0423055125903197,-1.9946452942262,
95.6335835610386));
#10585=CARTESIAN_POINT('Ctrl Pts',(-0.100292991783385,-1.99502164075874,
95.6241245703117));
#10586=CARTESIAN_POINT('Ctrl Pts',(-0.205692103694485,-1.98692107220505,
95.6168771600717));
#10587=CARTESIAN_POINT('Ctrl Pts',(-0.438786193166679,-1.95025783748678,
95.6004550758324));
#10588=CARTESIAN_POINT('Ctrl Pts',(-0.565338239443567,-1.91740336876445,
95.5912619438001));
#10589=CARTESIAN_POINT('Ctrl Pts',(-0.70875251942594,-1.86472424447827,
95.5810553193265));
#10590=CARTESIAN_POINT('Ctrl Pts',(-0.729592858535322,-1.85666933080406,
95.5795782814347));
#10591=CARTESIAN_POINT('Ctrl Pts',(-0.761913460968846,-1.84354893822585,
95.5773020214592));
#10592=CARTESIAN_POINT('Ctrl Pts',(-0.773488073689845,-1.83872266267815,
95.5764897838792));
#10593=CARTESIAN_POINT('Ctrl Pts',(-0.798145916596024,-1.82816701133072,
95.574766936133));
#10594=CARTESIAN_POINT('Ctrl Pts',(-0.811214793022019,-1.82240558457939,
95.5738583794762));
#10595=CARTESIAN_POINT('Ctrl Pts',(-0.846294315449824,-1.80648859104071,
95.5714290414359));
#10596=CARTESIAN_POINT('Ctrl Pts',(-0.868184277564329,-1.79607106809063,
95.5699232070324));
#10597=CARTESIAN_POINT('Ctrl Pts',(-0.96158028868379,-1.74951683809526,
95.5635191710709));
#10598=CARTESIAN_POINT('Ctrl Pts',(-1.03106959325041,-1.70948641136204,
95.5588058907052));
#10599=CARTESIAN_POINT('Ctrl Pts',(-1.23182815515036,-1.57712837923862,
95.544800178572));
#10600=CARTESIAN_POINT('Ctrl Pts',(-1.35454787343886,-1.47306851679111,
95.5356497288283));
#10601=CARTESIAN_POINT('Ctrl Pts',(-1.48619548145103,-1.33092723532978,
95.5238218625293));
#10602=CARTESIAN_POINT('Ctrl Pts',(-1.50828230089145,-1.30584402316266,
95.5217585561656));
#10603=CARTESIAN_POINT('Ctrl Pts',(-1.54501198392521,-1.26195589485126,
95.5181798524091));
#10604=CARTESIAN_POINT('Ctrl Pts',(-1.55996738582723,-1.24342124259173,
95.5166776770877));
#10605=CARTESIAN_POINT('Ctrl Pts',(-1.5901123428049,-1.20466170759963,95.5135522762242));
#10606=CARTESIAN_POINT('Ctrl Pts',(-1.60525616557102,-1.1844068715559,95.5119276036378));
#10607=CARTESIAN_POINT('Ctrl Pts',(-1.64437077414544,-1.12996260534527,
95.5075802533079));
#10608=CARTESIAN_POINT('Ctrl Pts',(-1.66765905954146,-1.09530067211596,
95.5048322861038));
#10609=CARTESIAN_POINT('Ctrl Pts',(-1.74232462677389,-0.976262348631661,
95.4954556278635));
#10610=CARTESIAN_POINT('Ctrl Pts',(-1.78851463349696,-0.88881631802061,
95.4886576921736));
#10611=CARTESIAN_POINT('Ctrl Pts',(-1.87821173646035,-0.683423136798174,
95.4730516775108));
#10612=CARTESIAN_POINT('Ctrl Pts',(-1.91744688388269,-0.564045799662935,
95.4642237314289));
#10613=CARTESIAN_POINT('Ctrl Pts',(-1.95048069896177,-0.418590018862053,
95.4542342277323));
#10614=CARTESIAN_POINT('Ctrl Pts',(-1.95533043058807,-0.395317072854785,
95.4526592277267));
#10615=CARTESIAN_POINT('Ctrl Pts',(-1.96240840658594,-0.358025186918168,
95.4501784518105));
#10616=CARTESIAN_POINT('Ctrl Pts',(-1.96490494315641,-0.344060150975849,
95.4492590037126));
#10617=CARTESIAN_POINT('Ctrl Pts',(-1.96963377948949,-0.315875703541852,
95.447424185483));
#10618=CARTESIAN_POINT('Ctrl Pts',(-1.97186158370587,-0.301656445141128,
95.4465090857984));
#10619=CARTESIAN_POINT('Ctrl Pts',(-1.97614996123957,-0.272204204994292,
95.4446331605963));
#10620=CARTESIAN_POINT('Ctrl Pts',(-1.97818875876497,-0.256968998038571,
95.4436735154417));
#10621=CARTESIAN_POINT('Ctrl Pts',(-1.98346971106087,-0.213708464554809,
95.4409751280481));
#10622=CARTESIAN_POINT('Ctrl Pts',(-1.98629384811802,-0.185634892351318,
95.4392554960969));
#10623=CARTESIAN_POINT('Ctrl Pts',(-1.99262757669528,-0.105672998812069,
95.4344229864603));
#10624=CARTESIAN_POINT('Ctrl Pts',(-1.99470520880076,-0.0536936062182133,
95.4313594480369));
#10625=CARTESIAN_POINT('Ctrl Pts',(-1.99474928355678,-0.00169063588936904,
95.428322530593));
#10626=CARTESIAN_POINT('Ctrl Pts',(-1.99474928174581,-0.00169277126666055,
95.4283226552967));
#10627=CARTESIAN_POINT('Ctrl Pts',(-1.99487747865361,0.149373527398597,
95.4195005439435));
#10628=CARTESIAN_POINT('Ctrl Pts',(-1.9778456373477,0.299964032517438,95.4109013801887));
#10629=CARTESIAN_POINT('Ctrl Pts',(-1.93456535897058,0.488105111933841,
95.399251979848));
#10630=CARTESIAN_POINT('Ctrl Pts',(-1.92386597454785,0.528705080201953,
95.3966854295853));
#10631=CARTESIAN_POINT('Ctrl Pts',(-1.90467016788025,0.593212163409328,
95.3925045977965));
#10632=CARTESIAN_POINT('Ctrl Pts',(-1.89698447461586,0.617348303740286,
95.3909167606056));
#10633=CARTESIAN_POINT('Ctrl Pts',(-1.88119219618946,0.663859583565867,
95.3878076720259));
#10634=CARTESIAN_POINT('Ctrl Pts',(-1.87314065820016,0.686248948327138,
95.3862884790016));
#10635=CARTESIAN_POINT('Ctrl Pts',(-1.85286969062847,0.7396007044466,95.3826115369586));
#10636=CARTESIAN_POINT('Ctrl Pts',(-1.84027232339096,0.770410829364629,
95.3804413789972));
#10637=CARTESIAN_POINT('Ctrl Pts',(-1.78193221943771,0.903490492294931,
95.3708557820111));
#10638=CARTESIAN_POINT('Ctrl Pts',(-1.72842993999459,1.00202919778739,95.3631863110547));
#10639=CARTESIAN_POINT('Ctrl Pts',(-1.66701714412024,1.09548226992006,95.3554060137221));
#10640=CARTESIAN_POINT('',(-1.99474996431002,-0.000377339601584004,95.2691777234731));
#10641=CARTESIAN_POINT('Ctrl Pts',(-1.66701720893993,1.09548217128264,95.1987207124569));
#10642=CARTESIAN_POINT('Ctrl Pts',(-1.66802828759705,1.09394359259538,95.1988441226394));
#10643=CARTESIAN_POINT('Ctrl Pts',(-1.66903726848786,1.09240356500824,95.1989674367045));
#10644=CARTESIAN_POINT('Ctrl Pts',(-1.68280203943216,1.07133052990688,95.2006518868572));
#10645=CARTESIAN_POINT('Ctrl Pts',(-1.69521699123801,1.05157561539804,95.2021966907627));
#10646=CARTESIAN_POINT('Ctrl Pts',(-1.71457241109769,1.01954287441436,95.2046416413902));
#10647=CARTESIAN_POINT('Ctrl Pts',(-1.72173395913149,1.00740182503062,95.2055548244644));
#10648=CARTESIAN_POINT('Ctrl Pts',(-1.73599476179255,0.982628952685094,
95.20738930547));
#10649=CARTESIAN_POINT('Ctrl Pts',(-1.74308623460031,0.969993753431862,
95.2083101336997));
#10650=CARTESIAN_POINT('Ctrl Pts',(-1.76216931572772,0.935107323861602,
95.210815275299));
#10651=CARTESIAN_POINT('Ctrl Pts',(-1.77387706730868,0.91270295973959,95.2123829817895));
#10652=CARTESIAN_POINT('Ctrl Pts',(-1.82499346896941,0.81018332385509,95.2193996423362));
#10653=CARTESIAN_POINT('Ctrl Pts',(-1.85942576560974,0.72769304324409,95.2246203371528));
#10654=CARTESIAN_POINT('Ctrl Pts',(-1.93427802862944,0.507940526652045,
95.2381069057587));
#10655=CARTESIAN_POINT('Ctrl Pts',(-1.96567577102525,0.368171235952138,
95.2463088270924));
#10656=CARTESIAN_POINT('Ctrl Pts',(-1.98591952037962,0.190843582955943,
95.2571576814379));
#10657=CARTESIAN_POINT('Ctrl Pts',(-1.98901186887296,0.155335634415854,
95.2593495024733));
#10658=CARTESIAN_POINT('Ctrl Pts',(-1.99250218417579,0.0973076913499925,
95.2629734686202));
#10659=CARTESIAN_POINT('Ctrl Pts',(-1.9934729078245,0.0748294058175734,
95.2643874976281));
#10660=CARTESIAN_POINT('Ctrl Pts',(-1.99452436434611,0.0347709085144968,
95.2669276932659));
#10661=CARTESIAN_POINT('Ctrl Pts',(-1.99475328875839,0.0171968647529458,
95.2680490325194));
#10662=CARTESIAN_POINT('Ctrl Pts',(-1.99474996431002,-0.000377339601584004,
95.2691777234731));
#10663=CARTESIAN_POINT('Ctrl Pts',(-1.66701720851842,1.09548217192407,95.9972028497351));
#10664=CARTESIAN_POINT('Ctrl Pts',(-1.6668804849266,1.09569022695793,95.9971884173542));
#10665=CARTESIAN_POINT('Ctrl Pts',(-1.66674372178711,1.09589825730506,95.9971739849087));
#10666=CARTESIAN_POINT('Ctrl Pts',(-1.60429633353987,1.19084822050707,95.9905858626106));
#10667=CARTESIAN_POINT('Ctrl Pts',(-1.53402745914654,1.2800937819193,95.9840334802001));
#10668=CARTESIAN_POINT('Ctrl Pts',(-1.44022506551533,1.38034473607148,95.9756036167107));
#10669=CARTESIAN_POINT('Ctrl Pts',(-1.42356866007336,1.39751636144373,95.974116948274));
#10670=CARTESIAN_POINT('Ctrl Pts',(-1.39653426673596,1.42440214384986,95.9717117554366));
#10671=CARTESIAN_POINT('Ctrl Pts',(-1.38635372287017,1.43431264182164,95.9708076996927));
#10672=CARTESIAN_POINT('Ctrl Pts',(-1.36567984616665,1.45401239274738,95.9689729904776));
#10673=CARTESIAN_POINT('Ctrl Pts',(-1.3551850454292,1.46379880526544,95.9680422534304));
#10674=CARTESIAN_POINT('Ctrl Pts',(-1.32642392666607,1.49004418302365,95.9654955061654));
#10675=CARTESIAN_POINT('Ctrl Pts',(-1.30795796645712,1.50627949837785,95.9638646203654));
#10676=CARTESIAN_POINT('Ctrl Pts',(-1.22578862674561,1.57587266525385,95.9566435479395));
#10677=CARTESIAN_POINT('Ctrl Pts',(-1.15909077817714,1.6255579711623,95.9508778893337));
#10678=CARTESIAN_POINT('Ctrl Pts',(-0.959697853330762,1.75556762473521,
95.9342790910101));
#10679=CARTESIAN_POINT('Ctrl Pts',(-0.820455885106113,1.82480295950729,
95.9234773012427));
#10680=CARTESIAN_POINT('Ctrl Pts',(-0.642417649259808,1.88878147799821,
95.9109795939836));
#10681=CARTESIAN_POINT('Ctrl Pts',(-0.609957156241353,1.89951267845743,
95.9087480327944));
#10682=CARTESIAN_POINT('Ctrl Pts',(-0.554553930603341,1.91626171340789,
95.9050159099953));
#10683=CARTESIAN_POINT('Ctrl Pts',(-0.53175156304769,1.92271406395186,95.9035014232127));
#10684=CARTESIAN_POINT('Ctrl Pts',(-0.484675213996757,1.93513359119853,
95.9004167556999));
#10685=CARTESIAN_POINT('Ctrl Pts',(-0.460393142552787,1.94105392090838,
95.8988483331189));
#10686=CARTESIAN_POINT('Ctrl Pts',(-0.396823108916739,1.95529313799269,
95.894796715629));
#10687=CARTESIAN_POINT('Ctrl Pts',(-0.357383000908921,1.96288500973171,
95.892336901338));
#10688=CARTESIAN_POINT('Ctrl Pts',(-0.204445405882167,1.98756109035315,
95.8829680732485));
#10689=CARTESIAN_POINT('Ctrl Pts',(-0.089783335550865,1.99603079495289,
95.8763155700666));
#10690=CARTESIAN_POINT('Ctrl Pts',(0.136881162197166,1.99319221518432,95.8631720438534));
#10691=CARTESIAN_POINT('Ctrl Pts',(0.248454710518279,1.98237641249894,95.8566996018982));
#10692=CARTESIAN_POINT('Ctrl Pts',(0.382100773166669,1.95795843928683,95.8483579931264));
#10693=CARTESIAN_POINT('Ctrl Pts',(0.40560224615661,1.9532252683376,95.8468682222481));
#10694=CARTESIAN_POINT('Ctrl Pts',(0.442905949010768,1.94501010341849,95.8444586424363));
#10695=CARTESIAN_POINT('Ctrl Pts',(0.456766826120236,1.94180174614435,95.8435533564393));
#10696=CARTESIAN_POINT('Ctrl Pts',(0.484535045439318,1.93506052268165,95.8417175132417));
#10697=CARTESIAN_POINT('Ctrl Pts',(0.498440916820015,1.93152531909679,95.840786887517));
#10698=CARTESIAN_POINT('Ctrl Pts',(0.536059543298598,1.92152849524061,95.8382409518977));
#10699=CARTESIAN_POINT('Ctrl Pts',(0.559692227728055,1.91477833469492,95.8366107833347));
#10700=CARTESIAN_POINT('Ctrl Pts',(0.662568301886348,1.88332688303307,95.8293968235987));
#10701=CARTESIAN_POINT('Ctrl Pts',(0.740345460910375,1.85413139794827,95.8236379340896));
#10702=CARTESIAN_POINT('Ctrl Pts',(0.957588248540831,1.75673137430935,95.8070363844033));
#10703=CARTESIAN_POINT('Ctrl Pts',(1.09124951906365,1.67698269264066,95.7962246606123));
#10704=CARTESIAN_POINT('Ctrl Pts',(1.24142742211929,1.56174646183854,95.7837200819162));
#10705=CARTESIAN_POINT('Ctrl Pts',(1.26798635304312,1.54026131022483,95.7814903549566));
#10706=CARTESIAN_POINT('Ctrl Pts',(1.31200921584522,1.50273766044407,95.7777605469953));
#10707=CARTESIAN_POINT('Ctrl Pts',(1.32976202831772,1.48705133968567,95.7762465732006));
#10708=CARTESIAN_POINT('Ctrl Pts',(1.36566198371057,1.45417312316325,95.77316238363));
#10709=CARTESIAN_POINT('Ctrl Pts',(1.38377389160839,1.43694886253776,95.7715939357578));
#10710=CARTESIAN_POINT('Ctrl Pts',(1.43014409775887,1.3911611513272,95.7675410770411));
#10711=CARTESIAN_POINT('Ctrl Pts',(1.45787227569515,1.36207571491972,95.7650800899108));
#10712=CARTESIAN_POINT('Ctrl Pts',(1.59088092058869,1.21383758313938,95.7530358693994));
#10713=CARTESIAN_POINT('Ctrl Pts',(1.68252649186866,1.08324029997221,95.744010236509));
#10714=CARTESIAN_POINT('Ctrl Pts',(1.79279399776592,0.877739634866055,95.7303674974415));
#10715=CARTESIAN_POINT('Ctrl Pts',(1.82420794422698,0.810432182841149,95.7259661528869));
#10716=CARTESIAN_POINT('Ctrl Pts',(1.85949243853509,0.722318552123517,95.7200990614011));
#10717=CARTESIAN_POINT('Ctrl Pts',(1.86688899986503,0.702980512553152,95.7188050892396));
#10718=CARTESIAN_POINT('Ctrl Pts',(1.87860176379632,0.670868590711476,95.7166404547415));
#10719=CARTESIAN_POINT('Ctrl Pts',(1.88309205089432,0.658159230235376,95.7157796159247));
#10720=CARTESIAN_POINT('Ctrl Pts',(1.89238911763242,0.630970457586125,95.7139276723563));
#10721=CARTESIAN_POINT('Ctrl Pts',(1.89715909993132,0.616480011172265,95.712934715081));
#10722=CARTESIAN_POINT('Ctrl Pts',(1.9105695639407,0.574110926068069,95.7100170163937));
#10723=CARTESIAN_POINT('Ctrl Pts',(1.91876460274693,0.54609669977558,95.7080699005966));
#10724=CARTESIAN_POINT('Ctrl Pts',(1.96162978023872,0.386663116313515,95.6969255419223));
#10725=CARTESIAN_POINT('Ctrl Pts',(1.98341032242802,0.252154077736425,95.6873117790037));
#10726=CARTESIAN_POINT('Ctrl Pts',(1.99707619038273,0.0185205112697676,
95.6710916348758));
#10727=CARTESIAN_POINT('Ctrl Pts',(1.9955708102381,-0.0797383823695557,
95.664407174551));
#10728=CARTESIAN_POINT('Ctrl Pts',(1.98394530854109,-0.209868232954295,
95.6557993807004));
#10729=CARTESIAN_POINT('Ctrl Pts',(1.98026285094011,-0.242162984086466,
95.6536824128717));
#10730=CARTESIAN_POINT('Ctrl Pts',(1.97253719478053,-0.297800008652776,
95.6500664284491));
#10731=CARTESIAN_POINT('Ctrl Pts',(1.96886450855976,-0.321186015878491,
95.6485560597808));
#10732=CARTESIAN_POINT('Ctrl Pts',(1.96035599414429,-0.369712087492614,
95.645439858646));
#10733=CARTESIAN_POINT('Ctrl Pts',(1.95545072718728,-0.394835664403702,
95.6438365433885));
#10734=CARTESIAN_POINT('Ctrl Pts',(1.94091771332892,-0.462335241306044,
95.6395511921536));
#10735=CARTESIAN_POINT('Ctrl Pts',(1.93038648945833,-0.504503579980473,
95.6368981879895));
#10736=CARTESIAN_POINT('Ctrl Pts',(1.89676002257848,-0.622593052559095,
95.629501754739));
#10737=CARTESIAN_POINT('Ctrl Pts',(1.8705012297357,-0.697529392975611,95.6248502118933));
#10738=CARTESIAN_POINT('Ctrl Pts',(1.78492443945544,-0.90182018466734,95.6119704544728));
#10739=CARTESIAN_POINT('Ctrl Pts',(1.71615061848828,-1.02667026181237,95.6038794510283));
#10740=CARTESIAN_POINT('Ctrl Pts',(1.62121697230445,-1.16242730818389,95.5937000511406));
#10741=CARTESIAN_POINT('Ctrl Pts',(1.60738681205321,-1.18147756659049,95.5922361474023));
#10742=CARTESIAN_POINT('Ctrl Pts',(1.58471715602143,-1.21156879558851,95.589858482816));
#10743=CARTESIAN_POINT('Ctrl Pts',(1.57609125577559,-1.22276888311434,95.5889585847402));
#10744=CARTESIAN_POINT('Ctrl Pts',(1.55841546156062,-1.24522179377426,95.5871220052268));
#10745=CARTESIAN_POINT('Ctrl Pts',(1.54936103552292,-1.25646982326632,95.586185073764));
#10746=CARTESIAN_POINT('Ctrl Pts',(1.5242786393232,-1.28694552053004,95.5836023242514));
#10747=CARTESIAN_POINT('Ctrl Pts',(1.50801009620147,-1.30597073284255,95.5819409575158));
#10748=CARTESIAN_POINT('Ctrl Pts',(1.4335927114004,-1.38975318888101,95.5744209048966));
#10749=CARTESIAN_POINT('Ctrl Pts',(1.37160457042969,-1.45096535589064,95.5683712483666));
#10750=CARTESIAN_POINT('Ctrl Pts',(1.19384786551966,-1.60489759793944,95.551966785172));
#10751=CARTESIAN_POINT('Ctrl Pts',(1.07139945953297,-1.68910811201298,95.5416575085761));
#10752=CARTESIAN_POINT('Ctrl Pts',(0.909785653747475,-1.77554210064671,
95.529533410311));
#10753=CARTESIAN_POINT('Ctrl Pts',(0.878399661951723,-1.79127719260074,
95.5272391271243));
#10754=CARTESIAN_POINT('Ctrl Pts',(0.825025261387033,-1.81629548886062,
95.5234350237021));
#10755=CARTESIAN_POINT('Ctrl Pts',(0.803257102718503,-1.82602686004232,
95.5219099663663));
#10756=CARTESIAN_POINT('Ctrl Pts',(0.758549468498303,-1.84505898753218,
95.5188291870527));
#10757=CARTESIAN_POINT('Ctrl Pts',(0.735600859048451,-1.85432775639869,
95.5172747705094));
#10758=CARTESIAN_POINT('Ctrl Pts',(0.676200430981533,-1.87704278709469,
95.5133160036981));
#10759=CARTESIAN_POINT('Ctrl Pts',(0.639516758065794,-1.88985588611785,
95.5109329363723));
#10760=CARTESIAN_POINT('Ctrl Pts',(0.557116277702242,-1.91596280864444,
95.5056968943315));
#10761=CARTESIAN_POINT('Ctrl Pts',(0.511250611400254,-1.92870818676769,
95.50286065405));
#10762=CARTESIAN_POINT('Ctrl Pts',(0.34568589476606,-1.96839407045617,95.4928223941057));
#10763=CARTESIAN_POINT('Ctrl Pts',(0.224022178038709,-1.98592222931546,
95.485829206451));
#10764=CARTESIAN_POINT('Ctrl Pts',(0.0353405790285169,-1.99553748330494,
95.4747343014208));
#10765=CARTESIAN_POINT('Ctrl Pts',(-0.0309608271509282,-1.99560981837558,
95.4707843446693));
#10766=CARTESIAN_POINT('Ctrl Pts',(-0.117408298304569,-1.99139518890504,
95.4654293578231));
#10767=CARTESIAN_POINT('Ctrl Pts',(-0.137663428620152,-1.99009753797934,
95.4641598526853));
#10768=CARTESIAN_POINT('Ctrl Pts',(-0.171401369062353,-1.98741860840557,
95.4620153507443));
#10769=CARTESIAN_POINT('Ctrl Pts',(-0.184896767081178,-1.98620853165765,
95.4611494532922));
#10770=CARTESIAN_POINT('Ctrl Pts',(-0.213792624288833,-1.98332050686113,
95.4592765458064));
#10771=CARTESIAN_POINT('Ctrl Pts',(-0.229187296533426,-1.9816005310061,
95.4582674983234));
#10772=CARTESIAN_POINT('Ctrl Pts',(-0.27476792319316,-1.97596978970285,
95.4552496695103));
#10773=CARTESIAN_POINT('Ctrl Pts',(-0.304884874318545,-1.97154736248637,
95.4532162706466));
#10774=CARTESIAN_POINT('Ctrl Pts',(-0.377172120157074,-1.95923675261806,
95.4482586963375));
#10775=CARTESIAN_POINT('Ctrl Pts',(-0.419211859057176,-1.95067385198253,
95.4453119885369));
#10776=CARTESIAN_POINT('Ctrl Pts',(-0.627629794158019,-1.9011736045099,
95.4304785449886));
#10777=CARTESIAN_POINT('Ctrl Pts',(-0.788559727426716,-1.84026406201591,
95.418385180547));
#10778=CARTESIAN_POINT('Ctrl Pts',(-0.975880102200488,-1.7402198818578,
95.4042271508111));
#10779=CARTESIAN_POINT('Ctrl Pts',(-1.01142920599408,-1.7198019016725,95.4015313578321));
#10780=CARTESIAN_POINT('Ctrl Pts',(-1.06773039546024,-1.68511465598701,
95.3972450359742));
#10781=CARTESIAN_POINT('Ctrl Pts',(-1.08888411246433,-1.67152358258132,
95.3956304868089));
#10782=CARTESIAN_POINT('Ctrl Pts',(-1.12961460845479,-1.6442531412768,95.3925117133335));
#10783=CARTESIAN_POINT('Ctrl Pts',(-1.14921373532863,-1.63061504560477,
95.3910062857853));
#10784=CARTESIAN_POINT('Ctrl Pts',(-1.19599410254259,-1.59680030433749,
95.3873983322278));
#10785=CARTESIAN_POINT('Ctrl Pts',(-1.22291627140408,-1.57627697709067,
95.3853096366637));
#10786=CARTESIAN_POINT('Ctrl Pts',(-1.34576153555728,-1.47758663335609,
95.3756961624452));
#10787=CARTESIAN_POINT('Ctrl Pts',(-1.43480305972305,-1.39128744985625,
95.3685066037472));
#10788=CARTESIAN_POINT('Ctrl Pts',(-1.59106580722298,-1.2087663827373,95.354575622804));
#10789=CARTESIAN_POINT('Ctrl Pts',(-1.6589394085242,-1.11378647911449,95.3478521061144));
#10790=CARTESIAN_POINT('Ctrl Pts',(-1.73021015981792,-0.992958130028485,
95.3392359144624));
#10791=CARTESIAN_POINT('Ctrl Pts',(-1.74192376921246,-0.972262572592298,
95.3377576908817));
#10792=CARTESIAN_POINT('Ctrl Pts',(-1.76002954836182,-0.938895510076941,
95.3353624551874));
#10793=CARTESIAN_POINT('Ctrl Pts',(-1.76666167076963,-0.926355928195318,
95.3344596740909));
#10794=CARTESIAN_POINT('Ctrl Pts',(-1.77974904771161,-0.900959399357691,
95.3326238232502));
#10795=CARTESIAN_POINT('Ctrl Pts',(-1.78620004066283,-0.888101286913282,
95.3316906067212));
#10796=CARTESIAN_POINT('Ctrl Pts',(-1.80337709674544,-0.852919678675461,
95.3291293717002));
#10797=CARTESIAN_POINT('Ctrl Pts',(-1.81382703857817,-0.830465093503172,
95.3274862070553));
#10798=CARTESIAN_POINT('Ctrl Pts',(-1.85814204097891,-0.730413272875547,
95.3201459128128));
#10799=CARTESIAN_POINT('Ctrl Pts',(-1.88746268593931,-0.650905271121404,
95.314267189847));
#10800=CARTESIAN_POINT('Ctrl Pts',(-1.95408120416242,-0.427397707683001,
95.2980005412358));
#10801=CARTESIAN_POINT('Ctrl Pts',(-1.98048680204003,-0.280691985162438,
95.2876463359679));
#10802=CARTESIAN_POINT('Ctrl Pts',(-1.99206761974544,-0.106596547266537,
95.2760856043113));
#10803=CARTESIAN_POINT('Ctrl Pts',(-1.99328212697559,-0.0807631774867131,
95.2743871290724));
#10804=CARTESIAN_POINT('Ctrl Pts',(-1.99449450571052,-0.0367390039569643,
95.2715208843643));
#10805=CARTESIAN_POINT('Ctrl Pts',(-1.99474651892921,-0.0185591628008082,
95.2703454385103));
#10806=CARTESIAN_POINT('Ctrl Pts',(-1.99474996418557,-0.000377996936292165,
95.26917776569));
#10807=CARTESIAN_POINT('Origin',(0.,0.,93.6863092095721));
#10808=CARTESIAN_POINT('',(-2.45049957974585,0.00143515344103661,91.0079011502938));
#10809=CARTESIAN_POINT('',(1.07552003335881,2.20186441631719,90.7500985735148));
#10810=CARTESIAN_POINT('Ctrl Pts',(-2.45049957974552,0.00143515400488855,
91.0079011502643));
#10811=CARTESIAN_POINT('Ctrl Pts',(-2.45045513469659,0.0773242734643422,
91.0039383691107));
#10812=CARTESIAN_POINT('Ctrl Pts',(-2.44688570781849,0.153113617481004,
90.9999755879572));
#10813=CARTESIAN_POINT('Ctrl Pts',(-2.43981706709049,0.228567121725641,
90.9960128068037));
#10814=CARTESIAN_POINT('Ctrl Pts',(-2.43225809680979,0.309254600140117,
90.9917751398856));
#10815=CARTESIAN_POINT('Ctrl Pts',(-2.42067817110913,0.389716438532518,
90.9875374729676));
#10816=CARTESIAN_POINT('Ctrl Pts',(-2.40509883718744,0.469520855084889,
90.9832998060496));
#10817=CARTESIAN_POINT('Ctrl Pts',(-2.38954194646292,0.549210307399057,
90.9790682438081));
#10818=CARTESIAN_POINT('Ctrl Pts',(-2.36999717910937,0.628243767924927,
90.9748366815665));
#10819=CARTESIAN_POINT('Ctrl Pts',(-2.3465378718612,0.706194212608052,90.970605119325));
#10820=CARTESIAN_POINT('Ctrl Pts',(-2.32300893032839,0.784376037672345,
90.9663609965332));
#10821=CARTESIAN_POINT('Ctrl Pts',(-2.29554222219168,0.861467938715433,
90.9621168737413));
#10822=CARTESIAN_POINT('Ctrl Pts',(-2.26426354690845,0.93704900626465,90.9578727509494));
#10823=CARTESIAN_POINT('Ctrl Pts',(-2.23313447742932,1.01226856980888,90.9536489277833));
#10824=CARTESIAN_POINT('Ctrl Pts',(-2.198229996004,1.08599128588063,90.9494251046172));
#10825=CARTESIAN_POINT('Ctrl Pts',(-2.15972356100008,1.15781880709425,90.9452012814511));
#10826=CARTESIAN_POINT('Ctrl Pts',(-2.1212303860275,1.22962159386587,90.9409789127959));
#10827=CARTESIAN_POINT('Ctrl Pts',(-2.07913793966161,1.29953007383443,90.9367565441406));
#10828=CARTESIAN_POINT('Ctrl Pts',(-2.03366625515513,1.36716926993086,90.9325341754853));
#10829=CARTESIAN_POINT('Ctrl Pts',(-1.98819640912799,1.43480573128665,90.9283119775459));
#10830=CARTESIAN_POINT('Ctrl Pts',(-1.93934785597698,1.50017270716457,90.9240897796065));
#10831=CARTESIAN_POINT('Ctrl Pts',(-1.88738391238524,1.5629242519295,90.9198675816671));
#10832=CARTESIAN_POINT('Ctrl Pts',(-1.83495328127442,1.62623936752298,90.9156074642215));
#10833=CARTESIAN_POINT('Ctrl Pts',(-1.77935131023484,1.68689145526741,90.9113473467759));
#10834=CARTESIAN_POINT('Ctrl Pts',(-1.72088874892593,1.74456073663836,90.9070872293303));
#10835=CARTESIAN_POINT('Ctrl Pts',(-1.6628652686989,1.80179689482945,90.9028591073521));
#10836=CARTESIAN_POINT('Ctrl Pts',(-1.60202441132498,1.8560946328778,90.8986309853739));
#10837=CARTESIAN_POINT('Ctrl Pts',(-1.5387043079605,1.90718098319582,90.8944028633957));
#10838=CARTESIAN_POINT('Ctrl Pts',(-1.4746654612688,1.95884721212195,90.8901267482164));
#10839=CARTESIAN_POINT('Ctrl Pts',(-1.40809112214727,2.00722839985949,90.8858506330371));
#10840=CARTESIAN_POINT('Ctrl Pts',(-1.33936071827131,2.0520875021187,90.8815745178577));
#10841=CARTESIAN_POINT('Ctrl Pts',(-1.27063031439535,2.09694660437791,90.8772984026784));
#10842=CARTESIAN_POINT('Ctrl Pts',(-1.19974429486011,2.13828343119256,90.8730222874991));
#10843=CARTESIAN_POINT('Ctrl Pts',(-1.12710540617508,2.17590984495473,90.8687461723198));
#10844=CARTESIAN_POINT('Ctrl Pts',(-1.05595631550261,2.21276455422834,90.8645577587561));
#10845=CARTESIAN_POINT('Ctrl Pts',(-0.982852107750259,2.24620109854361,
90.8603693451924));
#10846=CARTESIAN_POINT('Ctrl Pts',(-0.90815856879314,2.27600489101575,90.8561809316287));
#10847=CARTESIAN_POINT('Ctrl Pts',(-0.83357144946631,2.3057662205303,90.8519984855079));
#10848=CARTESIAN_POINT('Ctrl Pts',(-0.757399931236271,2.33190489769667,
90.847816039387));
#10849=CARTESIAN_POINT('Ctrl Pts',(-0.680034221161387,2.35425226092053,
90.8436335932661));
#10850=CARTESIAN_POINT('Ctrl Pts',(-0.602755438791394,2.37657451476461,
90.8394558465198));
#10851=CARTESIAN_POINT('Ctrl Pts',(-0.524285584084021,2.39511378547164,
90.8352780997734));
#10852=CARTESIAN_POINT('Ctrl Pts',(-0.445033163404528,2.40975013921986,
90.831100353027));
#10853=CARTESIAN_POINT('Ctrl Pts',(-0.365828226585273,2.42437772363878,
90.8269251093656));
#10854=CARTESIAN_POINT('Ctrl Pts',(-0.285842120195265,2.43510694459348,
90.8227498657042));
#10855=CARTESIAN_POINT('Ctrl Pts',(-0.205495493448251,2.44186851656113,
90.8185746220427));
#10856=CARTESIAN_POINT('Ctrl Pts',(-0.125171178618621,2.44862821086894,
90.8144005378288));
#10857=CARTESIAN_POINT('Ctrl Pts',(-0.0444870154651063,2.45142240394326,
90.8102264536148));
#10858=CARTESIAN_POINT('Ctrl Pts',(0.036130810748099,2.45023362447639,90.8060523694009));
#10859=CARTESIAN_POINT('Ctrl Pts',(0.11675216395715,2.44904479300091,90.8018781025725));
#10860=CARTESIAN_POINT('Ctrl Pts',(0.197306699372924,2.44387265252368,90.7977038357441));
#10861=CARTESIAN_POINT('Ctrl Pts',(0.277369399422697,2.43475182847532,90.7935295689157));
#10862=CARTESIAN_POINT('Ctrl Pts',(0.357510268542577,2.42562209932714,90.7893512265496));
#10863=CARTESIAN_POINT('Ctrl Pts',(0.437157871055443,2.41253604661732,90.7851728841834));
#10864=CARTESIAN_POINT('Ctrl Pts',(0.51589427676123,2.39557996009422,90.7809945418173));
#10865=CARTESIAN_POINT('Ctrl Pts',(0.594674132214892,2.37861451655668,90.7768138936827));
#10866=CARTESIAN_POINT('Ctrl Pts',(0.672541331726469,2.3577749134305,90.7726332455481));
#10867=CARTESIAN_POINT('Ctrl Pts',(0.749092534027391,2.33319751102739,90.7684525974135));
#10868=CARTESIAN_POINT('Ctrl Pts',(0.825765885523192,2.3085808916058,90.764265278413));
#10869=CARTESIAN_POINT('Ctrl Pts',(0.901118605741132,2.2802147391212,90.7600779594125));
#10870=CARTESIAN_POINT('Ctrl Pts',(0.974767401018496,2.24828351502021,90.755890640412));
#10871=CARTESIAN_POINT('Ctrl Pts',(1.00872538615526,2.23356066681426,90.7539599514462));
#10872=CARTESIAN_POINT('Ctrl Pts',(1.0423214721646,2.21808054542054,90.7520292624805));
#10873=CARTESIAN_POINT('Ctrl Pts',(1.07552003335881,2.20186441631719,90.7500985735148));
#10874=CARTESIAN_POINT('',(-1.07508846035167,2.2020751695659,90.7500736540522));
#10875=CARTESIAN_POINT('Origin',(0.,0.,90.7500736540522));
#10876=CARTESIAN_POINT('',(-2.45072924584278,0.0021129184388593,90.8922461578402));
#10877=CARTESIAN_POINT('Ctrl Pts',(-1.07508846035167,2.2020751695659,90.7500736540522));
#10878=CARTESIAN_POINT('Ctrl Pts',(-1.8087830660249,1.84387368085965,90.7924958655468));
#10879=CARTESIAN_POINT('Ctrl Pts',(-2.40530016291556,1.0047114134998,90.8398867001428));
#10880=CARTESIAN_POINT('Ctrl Pts',(-2.45341561407347,0.0973545315146867,
90.8872775347387));
#10881=CARTESIAN_POINT('Ctrl Pts',(-2.45268413588137,0.00211460386502969,
90.8922461578402));
#10882=CARTESIAN_POINT('',(-2.45049967807228,0.00125609221652004,91.6922461578137));
#10883=CARTESIAN_POINT('Ctrl Pts',(-2.45049908924981,0.002112720007266,
90.8922461578402));
#10884=CARTESIAN_POINT('Ctrl Pts',(-2.45056743907129,-0.0771647870499678,
90.8963857471584));
#10885=CARTESIAN_POINT('Ctrl Pts',(-2.4467845025604,-0.156615417674207,
90.9005253364765));
#10886=CARTESIAN_POINT('Ctrl Pts',(-2.43912640173371,-0.235823337194504,
90.9046649257947));
#10887=CARTESIAN_POINT('Ctrl Pts',(-2.43142267969008,-0.315503118049918,
90.9088291756791));
#10888=CARTESIAN_POINT('Ctrl Pts',(-2.41979738988535,-0.394936793730064,
90.9129934255634));
#10889=CARTESIAN_POINT('Ctrl Pts',(-2.40427949190856,-0.473698611764804,
90.9171576754478));
#10890=CARTESIAN_POINT('Ctrl Pts',(-2.38888912154466,-0.551813157426998,
90.9212877031168));
#10891=CARTESIAN_POINT('Ctrl Pts',(-2.36966996403225,-0.629266359954761,
90.9254177307857));
#10892=CARTESIAN_POINT('Ctrl Pts',(-2.34670224663734,-0.705647798570415,
90.9295477584547));
#10893=CARTESIAN_POINT('Ctrl Pts',(-2.32374575456158,-0.781991906265813,
90.9336757676001));
#10894=CARTESIAN_POINT('Ctrl Pts',(-2.29704447515276,-0.857264824312452,
90.9378037767455));
#10895=CARTESIAN_POINT('Ctrl Pts',(-2.26672915922954,-0.931068831343059,
90.9419317858909));
#10896=CARTESIAN_POINT('Ctrl Pts',(-2.23641852515404,-1.00486144020376,
90.9460591575133));
#10897=CARTESIAN_POINT('Ctrl Pts',(-2.20249514766258,-1.07718513927766,
90.9501865291357));
#10898=CARTESIAN_POINT('Ctrl Pts',(-2.16513821012427,-1.14766144008583,
90.9543139007582));
#10899=CARTESIAN_POINT('Ctrl Pts',(-2.12720459960284,-1.21922567211385,
90.9585049859466));
#10900=CARTESIAN_POINT('Ctrl Pts',(-2.08573073865029,-1.28888451711404,
90.9626960711351));
#10901=CARTESIAN_POINT('Ctrl Pts',(-2.04095207066785,-1.35626874004993,
90.9668871563235));
#10902=CARTESIAN_POINT('Ctrl Pts',(-1.99679743076912,-1.42271390764082,
90.9710198352445));
#10903=CARTESIAN_POINT('Ctrl Pts',(-1.94942986193507,-1.48694709560799,
90.9751525141655));
#10904=CARTESIAN_POINT('Ctrl Pts',(-1.89911681959994,-1.54864636231536,
90.9792851930865));
#10905=CARTESIAN_POINT('Ctrl Pts',(-1.84773718206216,-1.61165360283673,
90.9835054814086));
#10906=CARTESIAN_POINT('Ctrl Pts',(-1.7932861136744,-1.67201785723896,90.9877257697308));
#10907=CARTESIAN_POINT('Ctrl Pts',(-1.73608761335537,-1.72943633845078,
90.991946058053));
#10908=CARTESIAN_POINT('Ctrl Pts',(-1.67888911303634,-1.7868548196626,90.9961663463752));
#10909=CARTESIAN_POINT('Ctrl Pts',(-1.61894362655612,-1.84132723005314,
91.0003866346973));
#10910=CARTESIAN_POINT('Ctrl Pts',(-1.55660843855108,-1.89259621130117,
91.0046069230195));
#10911=CARTESIAN_POINT('Ctrl Pts',(-1.49409889418781,-1.94400859586838,
91.0088390158156));
#10912=CARTESIAN_POINT('Ctrl Pts',(-1.42892132213003,-1.99241796493926,
91.0130711086118));
#10913=CARTESIAN_POINT('Ctrl Pts',(-1.36139612885017,-2.03753547953202,
91.0173032014079));
#10914=CARTESIAN_POINT('Ctrl Pts',(-1.29396893282173,-2.08258751645332,
91.0215291522969));
#10915=CARTESIAN_POINT('Ctrl Pts',(-1.22420126527627,-2.12435693113119,
91.025755103186));
#10916=CARTESIAN_POINT('Ctrl Pts',(-1.15244672085264,-2.16259492406599,
91.029981054075));
#10917=CARTESIAN_POINT('Ctrl Pts',(-1.08035988608247,-2.20100999450893,
91.0342265750512));
#10918=CARTESIAN_POINT('Ctrl Pts',(-1.00626809011726,-2.23586054731741,
91.0384720960274));
#10919=CARTESIAN_POINT('Ctrl Pts',(-0.930559563531785,-2.26693827633651,
91.0427176170036));
#10920=CARTESIAN_POINT('Ctrl Pts',(-0.855338954235491,-2.29781571931148,
91.0469357769521));
#10921=CARTESIAN_POINT('Ctrl Pts',(-0.778522825667158,-2.32496864381566,
91.0511539369007));
#10922=CARTESIAN_POINT('Ctrl Pts',(-0.700515124397133,-2.34823951301627,
91.0553720968493));
#10923=CARTESIAN_POINT('Ctrl Pts',(-0.622534457104597,-2.37150231757526,
91.0595887949724));
#10924=CARTESIAN_POINT('Ctrl Pts',(-0.543363482118892,-2.39088560576755,
91.0638054930955));
#10925=CARTESIAN_POINT('Ctrl Pts',(-0.463422411726648,-2.40628134645753,
91.0680221912187));
#10926=CARTESIAN_POINT('Ctrl Pts',(-0.383484579401404,-2.42167646353264,
91.0722387185416));
#10927=CARTESIAN_POINT('Ctrl Pts',(-0.302777170206746,-2.43308426730393,
91.0764552458646));
#10928=CARTESIAN_POINT('Ctrl Pts',(-0.221730309608513,-2.44044789327716,
91.0806717731875));
#10929=CARTESIAN_POINT('Ctrl Pts',(-0.139716850862543,-2.44789934087819,
91.0849385885471));
#10930=CARTESIAN_POINT('Ctrl Pts',(-0.0573562728661285,-2.45120944097674,
91.0892054039068));
#10931=CARTESIAN_POINT('Ctrl Pts',(0.0249025668580095,-2.45037346381401,
91.0934722192664));
#10932=CARTESIAN_POINT('Ctrl Pts',(0.106307188240684,-2.44954616787057,
91.0976947258083));
#10933=CARTESIAN_POINT('Ctrl Pts',(0.187611708700424,-2.44465859566981,
91.1019172323501));
#10934=CARTESIAN_POINT('Ctrl Pts',(0.268385105960193,-2.43575854404716,
91.106139738892));
#10935=CARTESIAN_POINT('Ctrl Pts',(0.350429895118906,-2.42671840355965,
91.1104287086605));
#10936=CARTESIAN_POINT('Ctrl Pts',(0.431926203475093,-2.41353845486016,
91.114717678429));
#10937=CARTESIAN_POINT('Ctrl Pts',(0.51243385038469,-2.39632255737409,91.1190066481976));
#10938=CARTESIAN_POINT('Ctrl Pts',(0.592941497294287,-2.37910665988803,
91.1232956179661));
#10939=CARTESIAN_POINT('Ctrl Pts',(0.672460020853889,-2.35785500412892,
91.1275845877346));
#10940=CARTESIAN_POINT('Ctrl Pts',(0.750567944672692,-2.33272330344381,
91.1318735575032));
#10941=CARTESIAN_POINT('Ctrl Pts',(0.827728943281444,-2.3078962817181,91.1361105308365));
#10942=CARTESIAN_POINT('Ctrl Pts',(0.903797115072659,-2.27919155039504,
91.1403475041698));
#10943=CARTESIAN_POINT('Ctrl Pts',(0.978355688278953,-2.24672437054753,
91.1445844775031));
#10944=CARTESIAN_POINT('Ctrl Pts',(1.05280945564194,-2.21430282931699,91.148815494988));
#10945=CARTESIAN_POINT('Ctrl Pts',(1.12575741783497,-2.17812952808982,91.1530465124729));
#10946=CARTESIAN_POINT('Ctrl Pts',(1.19679876863617,-2.13836922849889,91.1572775299578));
#10947=CARTESIAN_POINT('Ctrl Pts',(1.26806276455654,-2.09848431927512,91.1615218075423));
#10948=CARTESIAN_POINT('Ctrl Pts',(1.33740773158128,-2.05499004088285,91.1657660851268));
#10949=CARTESIAN_POINT('Ctrl Pts',(1.40445014968875,-2.0081010998053,91.1700103627114));
#10950=CARTESIAN_POINT('Ctrl Pts',(1.47116663636426,-1.96144011261336,91.1742340064419));
#10951=CARTESIAN_POINT('Ctrl Pts',(1.53560252560777,-1.91141765803171,91.1784576501724));
#10952=CARTESIAN_POINT('Ctrl Pts',(1.59740686925234,-1.85828995155907,91.1826812939028));
#10953=CARTESIAN_POINT('Ctrl Pts',(1.65919194304514,-1.80517880966699,91.186903620752));
#10954=CARTESIAN_POINT('Ctrl Pts',(1.71834674956607,-1.74896464061557,91.1911259476011));
#10955=CARTESIAN_POINT('Ctrl Pts',(1.77455333156267,-1.6899440000899,91.1953482744502));
#10956=CARTESIAN_POINT('Ctrl Pts',(1.83075947177766,-1.63092382346423,91.199570568112));
#10957=CARTESIAN_POINT('Ctrl Pts',(1.88401711481614,-1.56909755566347,91.2037928617738));
#10958=CARTESIAN_POINT('Ctrl Pts',(1.9340460977904,-1.50479764141951,91.2080151554355));
#10959=CARTESIAN_POINT('Ctrl Pts',(1.98452682754016,-1.43991711815258,91.2122755751481));
#10960=CARTESIAN_POINT('Ctrl Pts',(2.03171998594613,-1.37251841771079,91.2165359948607));
#10961=CARTESIAN_POINT('Ctrl Pts',(2.07538130018495,-1.30297456185554,91.2207964145733));
#10962=CARTESIAN_POINT('Ctrl Pts',(2.11871604921364,-1.23395085992365,91.2250249684367));
#10963=CARTESIAN_POINT('Ctrl Pts',(2.15857143470742,-1.16281442289989,91.2292535223));
#10964=CARTESIAN_POINT('Ctrl Pts',(2.19475485581178,-1.08995475726775,91.2334820761633));
#10965=CARTESIAN_POINT('Ctrl Pts',(2.23134728747168,-1.01627149974169,91.2377584288005));
#10966=CARTESIAN_POINT('Ctrl Pts',(2.26418402344729,-0.940826257024861,
91.2420347814378));
#10967=CARTESIAN_POINT('Ctrl Pts',(2.29311657414475,-0.864040871361226,
91.246311134075));
#10968=CARTESIAN_POINT('Ctrl Pts',(2.3220491248422,-0.78725548569759,91.2505874867123));
#10969=CARTESIAN_POINT('Ctrl Pts',(2.34707740405044,-0.709130436852748,
91.2548638393495));
#10970=CARTESIAN_POINT('Ctrl Pts',(2.36810573449615,-0.630099579627262,
91.2591401919867));
#10971=CARTESIAN_POINT('Ctrl Pts',(2.38888774293271,-0.551994475379956,
91.2633664522129));
#10972=CARTESIAN_POINT('Ctrl Pts',(2.40584138049712,-0.472710168724586,
91.267592712439));
#10973=CARTESIAN_POINT('Ctrl Pts',(2.41883666287613,-0.39265690917934,91.2718189726651));
#10974=CARTESIAN_POINT('Ctrl Pts',(2.43181305628693,-0.31272000905053,91.2760390899163));
#10975=CARTESIAN_POINT('Ctrl Pts',(2.44084244652806,-0.232016831806835,
91.2802592071674));
#10976=CARTESIAN_POINT('Ctrl Pts',(2.44584503305822,-0.150971269665648,
91.2844793244185));
#10977=CARTESIAN_POINT('Ctrl Pts',(2.45087946218339,-0.0694098341860879,
91.2887263036707));
#10978=CARTESIAN_POINT('Ctrl Pts',(2.45183551013241,0.0124978994752909,
91.2929732829228));
#10979=CARTESIAN_POINT('Ctrl Pts',(2.44868447964768,0.0943110233884802,
91.297220262175));
#10980=CARTESIAN_POINT('Ctrl Pts',(2.44555912884175,0.175457402008593,91.3014326301901));
#10981=CARTESIAN_POINT('Ctrl Pts',(2.43839341430412,0.256510233847653,91.3056449982052));
#10982=CARTESIAN_POINT('Ctrl Pts',(2.42721154767961,0.337037613347162,91.3098573662203));
#10983=CARTESIAN_POINT('Ctrl Pts',(2.41603348499446,0.417537598380396,91.3140683012374));
#10984=CARTESIAN_POINT('Ctrl Pts',(2.40084204720005,0.497512024633151,91.3182792362545));
#10985=CARTESIAN_POINT('Ctrl Pts',(2.38171323801658,0.576534736036415,91.3224901712716));
#10986=CARTESIAN_POINT('Ctrl Pts',(2.36258503746332,0.655554933137372,91.3267009723074));
#10987=CARTESIAN_POINT('Ctrl Pts',(2.33951982525727,0.733623022717624,91.3309117733433));
#10988=CARTESIAN_POINT('Ctrl Pts',(2.31264426668479,0.810325086474536,91.3351225743791));
#10989=CARTESIAN_POINT('Ctrl Pts',(2.28536733233596,0.888172665042057,91.3393962620534));
#10990=CARTESIAN_POINT('Ctrl Pts',(2.25416544730402,0.964612606952473,91.3436699497276));
#10991=CARTESIAN_POINT('Ctrl Pts',(2.2192221583429,1.03923205393208,91.3479436374019));
#10992=CARTESIAN_POINT('Ctrl Pts',(2.18474293714266,1.11286051006029,91.3521605679497));
#10993=CARTESIAN_POINT('Ctrl Pts',(2.14662137229914,1.18471614940506,91.3563774984976));
#10994=CARTESIAN_POINT('Ctrl Pts',(2.10507981829468,1.25442784113254,91.3605944290454));
#10995=CARTESIAN_POINT('Ctrl Pts',(2.06269958107988,1.32554694350742,91.3648964952829));
#10996=CARTESIAN_POINT('Ctrl Pts',(2.01676003344093,1.39443415560823,91.3691985615204));
#10997=CARTESIAN_POINT('Ctrl Pts',(1.96754200890561,1.46072882260592,91.3735006277579));
#10998=CARTESIAN_POINT('Ctrl Pts',(1.91832398437029,1.52702348960362,91.3778026939954));
#10999=CARTESIAN_POINT('Ctrl Pts',(1.86582785852188,1.59072526320331,91.3821047602329));
#11000=CARTESIAN_POINT('Ctrl Pts',(1.81037443843145,1.65151283454717,91.3864068264704));
#11001=CARTESIAN_POINT('Ctrl Pts',(1.75584060816807,1.71129235927951,91.3906375510964));
#11002=CARTESIAN_POINT('Ctrl Pts',(1.69823993396493,1.76848049263467,91.3948682757225));
#11003=CARTESIAN_POINT('Ctrl Pts',(1.63784841461398,1.8227459561734,91.3990990003486));
#11004=CARTESIAN_POINT('Ctrl Pts',(1.57754383172299,1.87693330200042,91.4033236346457));
#11005=CARTESIAN_POINT('Ctrl Pts',(1.51445672572685,1.92820602577567,91.4075482689428));
#11006=CARTESIAN_POINT('Ctrl Pts',(1.44890163164046,1.97626777331151,91.4117729032399));
#11007=CARTESIAN_POINT('Ctrl Pts',(1.38301722427066,2.02457095703332,91.4160187598113));
#11008=CARTESIAN_POINT('Ctrl Pts',(1.31464028193079,2.06963045947639,91.4202646163827));
#11009=CARTESIAN_POINT('Ctrl Pts',(1.24412577577074,2.11118481049454,91.4245104729541));
#11010=CARTESIAN_POINT('Ctrl Pts',(1.17409084086693,2.15245654913396,91.4287274533286));
#11011=CARTESIAN_POINT('Ctrl Pts',(1.10194773272879,2.19027042611534,91.432944433703));
#11012=CARTESIAN_POINT('Ctrl Pts',(1.02807379065457,2.22441330039387,91.4371614140775));
#11013=CARTESIAN_POINT('Ctrl Pts',(0.954224502422788,2.258544780221,91.4413769871252));
#11014=CARTESIAN_POINT('Ctrl Pts',(0.878645949137833,2.28900749525625,91.445592560173));
#11015=CARTESIAN_POINT('Ctrl Pts',(0.801738584013049,2.31563500856779,91.4498081332208));
#11016=CARTESIAN_POINT('Ctrl Pts',(0.724833307421517,2.34226179876983,91.4540235917884));
#11017=CARTESIAN_POINT('Ctrl Pts',(0.646599730549771,2.36505344316696,91.4582390503561));
#11018=CARTESIAN_POINT('Ctrl Pts',(0.567455362713911,2.38389275373856,91.4624545089237));
#11019=CARTESIAN_POINT('Ctrl Pts',(0.487319921642071,2.4029679766941,91.4667227549262));
#11020=CARTESIAN_POINT('Ctrl Pts',(0.406251190842225,2.41799106019703,91.4709910009288));
#11021=CARTESIAN_POINT('Ctrl Pts',(0.324693356818091,2.42889367285565,91.4752592469313));
#11022=CARTESIAN_POINT('Ctrl Pts',(0.24402705096861,2.43967710644975,91.4794808357167));
#11023=CARTESIAN_POINT('Ctrl Pts',(0.162882757072662,2.44642973684538,91.4837024245022));
#11024=CARTESIAN_POINT('Ctrl Pts',(0.0816936827292237,2.44913788754372,
91.4879240132876));
#11025=CARTESIAN_POINT('Ctrl Pts',(-0.000841350372748101,2.45189093417396,
91.4922155878987));
#11026=CARTESIAN_POINT('Ctrl Pts',(-0.0834221605331062,2.45046419170395,
91.4965071625098));
#11027=CARTESIAN_POINT('Ctrl Pts',(-0.165597476810826,2.4448983057939,91.5007987371208));
#11028=CARTESIAN_POINT('Ctrl Pts',(-0.247772793088547,2.43933241988385,
91.5050903117319));
#11029=CARTESIAN_POINT('Ctrl Pts',(-0.329542129134761,2.42962751502606,
91.509381886343));
#11030=CARTESIAN_POINT('Ctrl Pts',(-0.410465475052023,2.41587837934576,
91.5136734609541));
#11031=CARTESIAN_POINT('Ctrl Pts',(-0.490245391315762,2.40232351602617,
91.5179043965293));
#11032=CARTESIAN_POINT('Ctrl Pts',(-0.569503016509799,2.38478706615771,
91.5221353321046));
#11033=CARTESIAN_POINT('Ctrl Pts',(-0.647810405818882,2.36332222265877,
91.5263662676798));
#11034=CARTESIAN_POINT('Ctrl Pts',(-0.726005377566023,2.34188819394493,
91.5305911293524));
#11035=CARTESIAN_POINT('Ctrl Pts',(-0.803252378057271,2.31653709402733,
91.534815991025));
#11036=CARTESIAN_POINT('Ctrl Pts',(-0.879132023708561,2.2873734139598,91.5390408526976));
#11037=CARTESIAN_POINT('Ctrl Pts',(-0.955387759304852,2.25806518700174,
91.5432866544784));
#11038=CARTESIAN_POINT('Ctrl Pts',(-1.03026207846466,2.22490655876264,91.5475324562593));
#11039=CARTESIAN_POINT('Ctrl Pts',(-1.10334318304459,2.18805486001358,91.5517782580401));
#11040=CARTESIAN_POINT('Ctrl Pts',(-1.17593277617475,2.15145100962399,91.5559955044207));
#11041=CARTESIAN_POINT('Ctrl Pts',(-1.24675278077154,2.11120382374383,91.5602127508014));
#11042=CARTESIAN_POINT('Ctrl Pts',(-1.31541988539227,2.06751560456375,91.564429997182));
#11043=CARTESIAN_POINT('Ctrl Pts',(-1.38406430308522,2.02384181953636,91.5686458502264));
#11044=CARTESIAN_POINT('Ctrl Pts',(-1.45055684129531,1.97672950827991,91.5728617032708));
#11045=CARTESIAN_POINT('Ctrl Pts',(-1.51454099345995,1.92642566145942,91.5770775563152));
#11046=CARTESIAN_POINT('Ctrl Pts',(-1.57852361556741,1.87612301755807,91.5812933085457));
#11047=CARTESIAN_POINT('Ctrl Pts',(-1.63999760600182,1.8226292780823,91.5855090607761));
#11048=CARTESIAN_POINT('Ctrl Pts',(-1.69863867736784,1.76623240083236,91.5897248130065));
#11049=CARTESIAN_POINT('Ctrl Pts',(-1.75800568290457,1.70913737091632,91.5939927532091));
#11050=CARTESIAN_POINT('Ctrl Pts',(-1.81446878279535,1.64906715546246,91.5982606934117));
#11051=CARTESIAN_POINT('Ctrl Pts',(-1.8677305025613,1.58635841467246,91.6025286336143));
#11052=CARTESIAN_POINT('Ctrl Pts',(-1.92041783061837,1.52432594533862,91.6067505469616));
#11053=CARTESIAN_POINT('Ctrl Pts',(-1.96997225921513,1.4597119979723,91.610972460309));
#11054=CARTESIAN_POINT('Ctrl Pts',(-2.0161481003516,1.39287367964529,91.6151943736563));
#11055=CARTESIAN_POINT('Ctrl Pts',(-2.06307904773308,1.32494236484367,91.6194853272865));
#11056=CARTESIAN_POINT('Ctrl Pts',(-2.1065196539566,1.25471370317424,91.6237762809168));
#11057=CARTESIAN_POINT('Ctrl Pts',(-2.14626030531889,1.18258908831955,91.628067234547));
#11058=CARTESIAN_POINT('Ctrl Pts',(-2.18600095668118,1.11046447346486,91.6323581881772));
#11059=CARTESIAN_POINT('Ctrl Pts',(-2.22204149530785,1.0364443813276,91.6366491418074));
#11060=CARTESIAN_POINT('Ctrl Pts',(-2.25422390054525,0.96094997591474,91.6409400954376));
#11061=CARTESIAN_POINT('Ctrl Pts',(-2.28939609327408,0.878442041608973,
91.645629684266));
#11062=CARTESIAN_POINT('Ctrl Pts',(-2.32007409940227,0.793908437648198,
91.6503192730944));
#11063=CARTESIAN_POINT('Ctrl Pts',(-2.34604528037445,0.707828928790533,
91.6550088619228));
#11064=CARTESIAN_POINT('Ctrl Pts',(-2.3719365489229,0.622014283598263,91.6596840210489));
#11065=CARTESIAN_POINT('Ctrl Pts',(-2.39314975910987,0.534663482575286,
91.6643591801751));
#11066=CARTESIAN_POINT('Ctrl Pts',(-2.40952050134751,0.446274807250013,
91.6690343393012));
#11067=CARTESIAN_POINT('Ctrl Pts',(-2.42580494861234,0.358352054497048,
91.6736848542955));
#11068=CARTESIAN_POINT('Ctrl Pts',(-2.43729772338479,0.269402608710182,
91.6783353692898));
#11069=CARTESIAN_POINT('Ctrl Pts',(-2.4438848934866,0.17993575905863,91.682985884284));
#11070=CARTESIAN_POINT('Ctrl Pts',(-2.44825709721058,0.120552550917064,
91.6860726421273));
#11071=CARTESIAN_POINT('Ctrl Pts',(-2.45046908401557,0.0609417786025406,
91.6891593999705));
#11072=CARTESIAN_POINT('Ctrl Pts',(-2.45049967807228,0.00125609221651381,
91.6922461578137));
#11073=CARTESIAN_POINT('',(-2.45049913396335,-0.00206020505177885,92.4922461578873));
#11074=CARTESIAN_POINT('Ctrl Pts',(-2.45049967807254,0.00125609170658984,
91.6922461578401));
#11075=CARTESIAN_POINT('Ctrl Pts',(-2.45054204849881,-0.081404047988421,
91.6965210828678));
#11076=CARTESIAN_POINT('Ctrl Pts',(-2.44639764250949,-0.164058934585186,
91.7007960078954));
#11077=CARTESIAN_POINT('Ctrl Pts',(-2.43809446303437,-0.246263353589474,
91.7050709329231));
#11078=CARTESIAN_POINT('Ctrl Pts',(-2.4297882751226,-0.328497557182675,
91.7093474068564));
#11079=CARTESIAN_POINT('Ctrl Pts',(-2.41732036322395,-0.410280524442328,
91.7136238807896));
#11080=CARTESIAN_POINT('Ctrl Pts',(-2.40077043863469,-0.49117364646101,
91.7179003547229));
#11081=CARTESIAN_POINT('Ctrl Pts',(-2.3841963819031,-0.572184722149131,
91.722183064363));
#11082=CARTESIAN_POINT('Ctrl Pts',(-2.36352851502258,-0.652302922682686,
91.726465774003));
#11083=CARTESIAN_POINT('Ctrl Pts',(-2.33889738497076,-0.731101410597003,
91.7307484836431));
#11084=CARTESIAN_POINT('Ctrl Pts',(-2.31424815295302,-0.80995780927467,
91.7350343407419));
#11085=CARTESIAN_POINT('Ctrl Pts',(-2.28563001059868,-0.887492144238603,
91.7393201978406));
#11086=CARTESIAN_POINT('Ctrl Pts',(-2.25322208313341,-0.963296680197705,
91.7436060549394));
#11087=CARTESIAN_POINT('Ctrl Pts',(-2.22074618234079,-1.03926021078992,
91.7479009013192));
#11088=CARTESIAN_POINT('Ctrl Pts',(-2.18446480815363,-1.11348628981486,
91.7521957476989));
#11089=CARTESIAN_POINT('Ctrl Pts',(-2.14460364977197,-1.18559075375305,
91.7564905940787));
#11090=CARTESIAN_POINT('Ctrl Pts',(-2.10835720421532,-1.25115659861646,
91.7603959726929));
#11091=CARTESIAN_POINT('Ctrl Pts',(-2.06915148962827,-1.31496829758165,
91.7643013513071));
#11092=CARTESIAN_POINT('Ctrl Pts',(-2.02718605476699,-1.37675958299125,
91.7682067299212));
#11093=CARTESIAN_POINT('Ctrl Pts',(-1.98172888403876,-1.44369221504108,
91.772437055736));
#11094=CARTESIAN_POINT('Ctrl Pts',(-1.93286753073307,-1.50849728424299,
91.7766673815508));
#11095=CARTESIAN_POINT('Ctrl Pts',(-1.88082792531648,-1.57080761563907,
91.7808977073656));
#11096=CARTESIAN_POINT('Ctrl Pts',(-1.82886321192093,-1.6330282740522,91.7851219451701));
#11097=CARTESIAN_POINT('Ctrl Pts',(-1.77372962606296,-1.69276097108578,
91.7893461829747));
#11098=CARTESIAN_POINT('Ctrl Pts',(-1.71569621861873,-1.74966760712353,
91.7935704207792));
#11099=CARTESIAN_POINT('Ctrl Pts',(-1.65736444256019,-1.80686681867748,
91.7978163767636));
#11100=CARTESIAN_POINT('Ctrl Pts',(-1.59610320588525,-1.86121043003094,
91.802062332748));
#11101=CARTESIAN_POINT('Ctrl Pts',(-1.53222666532007,-1.91238900229062,
91.8063082887324));
#11102=CARTESIAN_POINT('Ctrl Pts',(-1.4687918697727,-1.96321364368439,91.8105248813561));
#11103=CARTESIAN_POINT('Ctrl Pts',(-1.40277819676894,-2.01091658948931,
91.8147414739798));
#11104=CARTESIAN_POINT('Ctrl Pts',(-1.33452872187373,-2.05523315964249,
91.8189580666035));
#11105=CARTESIAN_POINT('Ctrl Pts',(-1.26630195816462,-2.09953498269508,
91.8231732560835));
#11106=CARTESIAN_POINT('Ctrl Pts',(-1.19584125982708,-2.14045241472924,
91.8273884455635));
#11107=CARTESIAN_POINT('Ctrl Pts',(-1.12351923302871,-2.17776371147436,
91.8316036350435));
#11108=CARTESIAN_POINT('Ctrl Pts',(-1.05119908926899,-2.21507403675039,
91.8358187147732));
#11109=CARTESIAN_POINT('Ctrl Pts',(-0.97701812728281,-2.24877820109266,
91.8400337945029));
#11110=CARTESIAN_POINT('Ctrl Pts',(-0.901372849030125,-2.27870077830138,
91.8442488742326));
#11111=CARTESIAN_POINT('Ctrl Pts',(-0.824765148011244,-2.30900405567004,
91.848517581747));
#11112=CARTESIAN_POINT('Ctrl Pts',(-0.746656054289783,-2.33542864332484,
91.8527862892613));
#11113=CARTESIAN_POINT('Ctrl Pts',(-0.667475684203846,-2.35784360401546,
91.8570549967757));
#11114=CARTESIAN_POINT('Ctrl Pts',(-0.589176057216373,-2.38000923748129,
91.8612762223867));
#11115=CARTESIAN_POINT('Ctrl Pts',(-0.509829340652844,-2.39825395685959,
91.8654974479976));
#11116=CARTESIAN_POINT('Ctrl Pts',(-0.429862314547043,-2.41250256798459,
91.8697186736086));
#11117=CARTESIAN_POINT('Ctrl Pts',(-0.348546040512666,-2.42699158956353,
91.8740111220747));
#11118=CARTESIAN_POINT('Ctrl Pts',(-0.266588829685823,-2.4373483447573,
91.8783035705407));
#11119=CARTESIAN_POINT('Ctrl Pts',(-0.184443459463732,-2.44354882502091,
91.8825960190068));
#11120=CARTESIAN_POINT('Ctrl Pts',(-0.102298089241641,-2.44974930528451,
91.8868884674728));
#11121=CARTESIAN_POINT('Ctrl Pts',(-0.0199650595547671,-2.45179356480318,
91.8911809159389));
#11122=CARTESIAN_POINT('Ctrl Pts',(0.0621063035833999,-2.44971285195943,
91.8954733644049));
#11123=CARTESIAN_POINT('Ctrl Pts',(0.14298947043929,-2.4476622628418,91.8997036685235));
#11124=CARTESIAN_POINT('Ctrl Pts',(0.223923433706141,-2.44159767315364,
91.9039339726421));
#11125=CARTESIAN_POINT('Ctrl Pts',(0.304477161884593,-2.43151062261523,
91.9081642767606));
#11126=CARTESIAN_POINT('Ctrl Pts',(0.384914985049505,-2.42143808586477,
91.9123884940913));
#11127=CARTESIAN_POINT('Ctrl Pts',(0.464973202064389,-2.40735464023245,
91.916612711422));
#11128=CARTESIAN_POINT('Ctrl Pts',(0.544221926826333,-2.38930382001985,
91.9208369287527));
#11129=CARTESIAN_POINT('Ctrl Pts',(0.623878580013838,-2.37116008420902,
91.9250828900084));
#11130=CARTESIAN_POINT('Ctrl Pts',(0.702716906930503,-2.34900802085591,
91.929328851264));
#11131=CARTESIAN_POINT('Ctrl Pts',(0.780306737278808,-2.32294460669154,
91.9335748125197));
#11132=CARTESIAN_POINT('Ctrl Pts',(0.857359574879215,-2.29706157524393,
91.9377913878314));
#11133=CARTESIAN_POINT('Ctrl Pts',(0.933180696082373,-2.26732131234926,
91.9420079631432));
#11134=CARTESIAN_POINT('Ctrl Pts',(1.00736195527359,-2.23386932049916,91.9462245384549));
#11135=CARTESIAN_POINT('Ctrl Pts',(1.08151855097934,-2.20042845063221,91.9504397118567));
#11136=CARTESIAN_POINT('Ctrl Pts',(1.15403594365693,-2.16327849348567,91.9546548852586));
#11137=CARTESIAN_POINT('Ctrl Pts',(1.22452614081644,-2.12261300769999,91.9588700586604));
#11138=CARTESIAN_POINT('Ctrl Pts',(1.29501452371866,-2.08194856855139,91.9630851235732));
#11139=CARTESIAN_POINT('Ctrl Pts',(1.36347541244613,-2.03776901403212,91.9673001884861));
#11140=CARTESIAN_POINT('Ctrl Pts',(1.42954685953016,-1.9903130473389,91.9715152533989));
#11141=CARTESIAN_POINT('Ctrl Pts',(1.49645949177866,-1.94225289749381,91.9757839821897));
#11142=CARTESIAN_POINT('Ctrl Pts',(1.56092100197455,-1.8908325881893,91.9800527109805));
#11143=CARTESIAN_POINT('Ctrl Pts',(1.62258868631153,-1.83634316102787,91.9843214397713));
#11144=CARTESIAN_POINT('Ctrl Pts',(1.68356995501418,-1.78246024917687,91.9885426538514));
#11145=CARTESIAN_POINT('Ctrl Pts',(1.74181899125051,-1.72557657784546,91.9927638679315));
#11146=CARTESIAN_POINT('Ctrl Pts',(1.79704179678401,-1.66601051335558,91.9969850820116));
#11147=CARTESIAN_POINT('Ctrl Pts',(1.85319699839329,-1.60543872008672,92.0012775681577));
#11148=CARTESIAN_POINT('Ctrl Pts',(1.90622251051549,-1.54209350109308,92.0055700543039));
#11149=CARTESIAN_POINT('Ctrl Pts',(1.95585333010915,-1.47634277899847,92.00986254045));
#11150=CARTESIAN_POINT('Ctrl Pts',(2.00548414970282,-1.41059205690386,92.0141550265961));
#11151=CARTESIAN_POINT('Ctrl Pts',(2.05172005205402,-1.3424362816015,92.0184475127423));
#11152=CARTESIAN_POINT('Ctrl Pts',(2.09434438701957,-1.27227034806272,92.0227399988884));
#11153=CARTESIAN_POINT('Ctrl Pts',(2.13634997159352,-1.20312296880493,92.0269701737402));
#11154=CARTESIAN_POINT('Ctrl Pts',(2.17500662817988,-1.13176262298302,92.031200348592));
#11155=CARTESIAN_POINT('Ctrl Pts',(2.21007417864682,-1.05854729458752,92.0354305234437));
#11156=CARTESIAN_POINT('Ctrl Pts',(2.24509125006682,-0.98543735821257,92.0396546090423));
#11157=CARTESIAN_POINT('Ctrl Pts',(2.27652927687386,-0.910478158374995,
92.0438786946408));
#11158=CARTESIAN_POINT('Ctrl Pts',(2.30419243730191,-0.834054831459353,
92.0481027802393));
#11159=CARTESIAN_POINT('Ctrl Pts',(2.33199907311781,-0.757235133836242,
92.0523487741199));
#11160=CARTESIAN_POINT('Ctrl Pts',(2.355991321361,-0.678936482874058,92.0565947680004));
#11161=CARTESIAN_POINT('Ctrl Pts',(2.37601814514858,-0.599573201473082,
92.0608407618809));
#11162=CARTESIAN_POINT('Ctrl Pts',(2.3959055669807,-0.5207623489913,92.0650572004083));
#11163=CARTESIAN_POINT('Ctrl Pts',(2.41188247855823,-0.440902097328574,
92.0692736389357));
#11164=CARTESIAN_POINT('Ctrl Pts',(2.42385059077933,-0.360414433088791,
92.073490077463));
#11165=CARTESIAN_POINT('Ctrl Pts',(2.43581471922367,-0.279953560449852,
92.0777051124817));
#11166=CARTESIAN_POINT('Ctrl Pts',(2.44377262978494,-0.198866149730817,
92.0819201475003));
#11167=CARTESIAN_POINT('Ctrl Pts',(2.44767735546206,-0.117583219713877,
92.086135182519));
#11168=CARTESIAN_POINT('Ctrl Pts',(2.45158197932559,-0.0363024091047066,
92.0903501076329));
#11169=CARTESIAN_POINT('Ctrl Pts',(2.45143360717036,0.0451734459503161,
92.0945650327469));
#11170=CARTESIAN_POINT('Ctrl Pts',(2.44723733078306,0.126410825571998,92.0987799578608));
#11171=CARTESIAN_POINT('Ctrl Pts',(2.44298732864705,0.2086883032809,92.1030488474867));
#11172=CARTESIAN_POINT('Ctrl Pts',(2.43458503926964,0.290720666427331,92.1073177371127));
#11173=CARTESIAN_POINT('Ctrl Pts',(2.42209000187813,0.372062189428047,92.1115866267386));
#11174=CARTESIAN_POINT('Ctrl Pts',(2.40973492603825,0.452492575837969,92.1158076989474));
#11175=CARTESIAN_POINT('Ctrl Pts',(2.39337848850781,0.532247072678141,92.1200287711562));
#11176=CARTESIAN_POINT('Ctrl Pts',(2.37312953875738,0.610906246716464,92.1242498433649));
#11177=CARTESIAN_POINT('Ctrl Pts',(2.35253651085689,0.690902028500942,92.1285426416995));
#11178=CARTESIAN_POINT('Ctrl Pts',(2.32791760380993,0.769764436858667,92.132835440034));
#11179=CARTESIAN_POINT('Ctrl Pts',(2.29943908779298,0.847071503197811,92.1371282383685));
#11180=CARTESIAN_POINT('Ctrl Pts',(2.27096057177603,0.924378569536955,92.1414210367031));
#11181=CARTESIAN_POINT('Ctrl Pts',(2.238622703912,1.00012986131522,92.1457138350376));
#11182=CARTESIAN_POINT('Ctrl Pts',(2.20264060816859,1.0739295140961,92.1500066333722));
#11183=CARTESIAN_POINT('Ctrl Pts',(2.16718280059893,1.14665384637717,92.1542368821705));
#11184=CARTESIAN_POINT('Ctrl Pts',(2.12805256397583,1.2177573626794,92.1584671309689));
#11185=CARTESIAN_POINT('Ctrl Pts',(2.08542120336568,1.28684445623893,92.1626973797673));
#11186=CARTESIAN_POINT('Ctrl Pts',(2.04285119845761,1.35583211860344,92.1669215403273));
#11187=CARTESIAN_POINT('Ctrl Pts',(1.99679031914875,1.42280872933492,92.1711457008873));
#11188=CARTESIAN_POINT('Ctrl Pts',(1.947456693669,1.48740131648583,92.1753698614473));
#11189=CARTESIAN_POINT('Ctrl Pts',(1.8978682960114,1.55232747721748,92.1796158367143));
#11190=CARTESIAN_POINT('Ctrl Pts',(1.84497345720986,1.61484448977382,92.1838618119814));
#11191=CARTESIAN_POINT('Ctrl Pts',(1.78903905334931,1.67460130048648,92.1881077872484));
#11192=CARTESIAN_POINT('Ctrl Pts',(1.73349273925385,1.73394350042237,92.1923243026583));
#11193=CARTESIAN_POINT('Ctrl Pts',(1.67494922751663,1.79056333542785,92.1965408180682));
#11194=CARTESIAN_POINT('Ctrl Pts',(1.61371037718443,1.84414995826458,92.2007573334782));
#11195=CARTESIAN_POINT('Ctrl Pts',(1.55249190279551,1.89771875127628,92.204972445931));
#11196=CARTESIAN_POINT('Ctrl Pts',(1.48858022051328,1.94825603017984,92.2091875583838));
#11197=CARTESIAN_POINT('Ctrl Pts',(1.42231253559508,1.99548923853001,92.2134026708367));
#11198=CARTESIAN_POINT('Ctrl Pts',(1.35604657149998,2.04272122033974,92.2176176738325));
#11199=CARTESIAN_POINT('Ctrl Pts',(1.28742510583333,2.08664903305199,92.2218326768284));
#11200=CARTESIAN_POINT('Ctrl Pts',(1.21681559436603,2.12704256170572,92.2260476798242));
#11201=CARTESIAN_POINT('Ctrl Pts',(1.14530489498446,2.16795163223308,92.2303164788268));
#11202=CARTESIAN_POINT('Ctrl Pts',(1.07175545809905,2.20523530393737,92.2345852778295));
#11203=CARTESIAN_POINT('Ctrl Pts',(0.99657439692856,2.23870268713522,92.2388540768321));
#11204=CARTESIAN_POINT('Ctrl Pts',(0.922232511514979,2.27179650528639,92.2430752272304));
#11205=CARTESIAN_POINT('Ctrl Pts',(0.84629570675226,2.30115869439306,92.2472963776287));
#11206=CARTESIAN_POINT('Ctrl Pts',(0.76917568667271,2.32665403810527,92.2515175280271));
#11207=CARTESIAN_POINT('Ctrl Pts',(0.690749863326335,2.35258107132008,92.2558101513319));
#11208=CARTESIAN_POINT('Ctrl Pts',(0.611100869247195,2.37450896412485,92.2601027746366));
#11209=CARTESIAN_POINT('Ctrl Pts',(0.53067350902201,2.39234944705456,92.2643953979414));
#11210=CARTESIAN_POINT('Ctrl Pts',(0.450246148796826,2.41018992998427,92.2686880212462));
#11211=CARTESIAN_POINT('Ctrl Pts',(0.369040925144304,2.42394298546787,92.2729806445509));
#11212=CARTESIAN_POINT('Ctrl Pts',(0.287507097297213,2.43357554207872,92.2772732678557));
#11213=CARTESIAN_POINT('Ctrl Pts',(0.207158160424407,2.44306811348724,92.2815035085796));
#11214=CARTESIAN_POINT('Ctrl Pts',(0.126187085558151,2.44859500635354,92.2857337493035));
#11215=CARTESIAN_POINT('Ctrl Pts',(0.0450192880203518,2.45008642984409,
92.2899639900274));
#11216=CARTESIAN_POINT('Ctrl Pts',(-0.0360316924424859,2.45157570687095,
92.294188142569));
#11217=CARTESIAN_POINT('Ctrl Pts',(-0.117278372142718,2.4490410406876,92.2984122951106));
#11218=CARTESIAN_POINT('Ctrl Pts',(-0.198289060329829,2.44246426761038,
92.3026364476522));
#11219=CARTESIAN_POINT('Ctrl Pts',(-0.279718302759078,2.4358535146185,92.3068824249309));
#11220=CARTESIAN_POINT('Ctrl Pts',(-0.36090863530143,2.42515870594721,92.3111284022095));
#11221=CARTESIAN_POINT('Ctrl Pts',(-0.441420445307773,2.41041453705878,
92.3153743794881));
#11222=CARTESIAN_POINT('Ctrl Pts',(-0.521373453947438,2.39577270175003,
92.3195908870789));
#11223=CARTESIAN_POINT('Ctrl Pts',(-0.600656865358687,2.37713762325674,
92.3238073946698));
#11224=CARTESIAN_POINT('Ctrl Pts',(-0.678845978104483,2.35459516435658,
92.3280239022606));
#11225=CARTESIAN_POINT('Ctrl Pts',(-0.757009076738581,2.33206020550371,
92.3322390069873));
#11226=CARTESIAN_POINT('Ctrl Pts',(-0.834078153080863,2.30562057658316,
92.336454111714));
#11227=CARTESIAN_POINT('Ctrl Pts',(-0.909641605973001,2.27541257768407,
92.3406692164407));
#11228=CARTESIAN_POINT('Ctrl Pts',(-0.98520309851335,2.24520536247474,92.3448842118145));
#11229=CARTESIAN_POINT('Ctrl Pts',(-1.05925861371348,2.21123014533049,92.3490992071882));
#11230=CARTESIAN_POINT('Ctrl Pts',(-1.13141589754081,2.17367162119579,92.3533142025619));
#11231=CARTESIAN_POINT('Ctrl Pts',(-1.20449441503888,2.13563358653601,92.3575830108767));
#11232=CARTESIAN_POINT('Ctrl Pts',(-1.27562544557686,2.09392030856426,92.3618518191915));
#11233=CARTESIAN_POINT('Ctrl Pts',(-1.34442828614813,2.04877105441403,92.3661206275063));
#11234=CARTESIAN_POINT('Ctrl Pts',(-1.4124628792332,2.00412593353385,92.3703417706196));
#11235=CARTESIAN_POINT('Ctrl Pts',(-1.47822067261861,1.95612151404289,92.3745629137329));
#11236=CARTESIAN_POINT('Ctrl Pts',(-1.54136531969538,1.90503102369498,92.3787840568463));
#11237=CARTESIAN_POINT('Ctrl Pts',(-1.60557951200315,1.85307516165161,92.3830766977618));
#11238=CARTESIAN_POINT('Ctrl Pts',(-1.66709083966827,1.79792805094266,92.3873693386773));
#11239=CARTESIAN_POINT('Ctrl Pts',(-1.72558454712129,1.73991615336378,92.3916619795928));
#11240=CARTESIAN_POINT('Ctrl Pts',(-1.78407825457432,1.6819042557849,92.3959546205083));
#11241=CARTESIAN_POINT('Ctrl Pts',(-1.83955405521674,1.62102798475228,92.4002472614238));
#11242=CARTESIAN_POINT('Ctrl Pts',(-1.89174122025013,1.55764739450446,92.4045399023394));
#11243=CARTESIAN_POINT('Ctrl Pts',(-1.94293841432775,1.49546911029234,92.408751113466));
#11244=CARTESIAN_POINT('Ctrl Pts',(-1.99116949696977,1.43063916186968,92.4129623245927));
#11245=CARTESIAN_POINT('Ctrl Pts',(-2.03614600671605,1.36347339150212,92.4171735357193));
#11246=CARTESIAN_POINT('Ctrl Pts',(-2.08106070506784,1.2963999273173,92.421378959362));
#11247=CARTESIAN_POINT('Ctrl Pts',(-2.12272944818328,1.22699739761737,92.4255843830046));
#11248=CARTESIAN_POINT('Ctrl Pts',(-2.16090346112967,1.15561519619543,92.4297898066472));
#11249=CARTESIAN_POINT('Ctrl Pts',(-2.19903697527135,1.08430872414048,92.4339907687565));
#11250=CARTESIAN_POINT('Ctrl Pts',(-2.2336828995433,1.01102716117391,92.4381917308658));
#11251=CARTESIAN_POINT('Ctrl Pts',(-2.26463614119372,0.936148170963978,
92.4423926929751));
#11252=CARTESIAN_POINT('Ctrl Pts',(-2.29556969780512,0.861316800834073,
92.4465909834384));
#11253=CARTESIAN_POINT('Ctrl Pts',(-2.32281505157425,0.784890451273078,
92.4507892739017));
#11254=CARTESIAN_POINT('Ctrl Pts',(-2.34621401464293,0.70726943062253,92.4549875643651));
#11255=CARTESIAN_POINT('Ctrl Pts',(-2.36960328362365,0.629680568021022,
92.459184115495));
#11256=CARTESIAN_POINT('Ctrl Pts',(-2.38914919410262,0.550898467200658,
92.463380666625));
#11257=CARTESIAN_POINT('Ctrl Pts',(-2.40474302292967,0.471339838832957,
92.467577217755));
#11258=CARTESIAN_POINT('Ctrl Pts',(-2.42034235417786,0.391753137495906,
92.4717752496753));
#11259=CARTESIAN_POINT('Ctrl Pts',(-2.43198671970401,0.311389820912447,
92.4759732815957));
#11260=CARTESIAN_POINT('Ctrl Pts',(-2.4396184727168,0.230677171776809,92.480171313516));
#11261=CARTESIAN_POINT('Ctrl Pts',(-2.44693557045041,0.153292285096926,
92.4841962616241));
#11262=CARTESIAN_POINT('Ctrl Pts',(-2.45056441392189,0.0755867030845429,
92.4882212097322));
#11263=CARTESIAN_POINT('Ctrl Pts',(-2.45049913396412,-0.00206020414336211,
92.4922461578402));
#11264=CARTESIAN_POINT('',(-2.45049997091768,-0.0003775346874681,93.2922461577912));
#11265=CARTESIAN_POINT('Ctrl Pts',(-2.45049913396335,-0.00206020505177728,
92.4922461578873));
#11266=CARTESIAN_POINT('Ctrl Pts',(-2.45041769687901,-0.0989250799796706,
92.497267299218));
#11267=CARTESIAN_POINT('Ctrl Pts',(-2.44458900316372,-0.195541487778647,
92.5022884405487));
#11268=CARTESIAN_POINT('Ctrl Pts',(-2.43312414260481,-0.291302517451572,
92.5073095818795));
#11269=CARTESIAN_POINT('Ctrl Pts',(-2.42151339890458,-0.388282046010988,
92.5123946140762));
#11270=CARTESIAN_POINT('Ctrl Pts',(-2.40412222586561,-0.484384242648835,
92.517479646273));
#11271=CARTESIAN_POINT('Ctrl Pts',(-2.38111506273585,-0.579000265986519,
92.5225646784698));
#11272=CARTESIAN_POINT('Ctrl Pts',(-2.36717683943469,-0.636320642849597,
92.5256452979209));
#11273=CARTESIAN_POINT('Ctrl Pts',(-2.35117837970355,-0.693095985603747,
92.528725917372));
#11274=CARTESIAN_POINT('Ctrl Pts',(-2.33316468060956,-0.74919478318798,
92.5318065368231));
#11275=CARTESIAN_POINT('Ctrl Pts',(-2.30842868017434,-0.82622837158192,
92.5360367731385));
#11276=CARTESIAN_POINT('Ctrl Pts',(-2.27982683123968,-0.902180851879758,
92.540267009454));
#11277=CARTESIAN_POINT('Ctrl Pts',(-2.24747233236836,-0.976636250217406,
92.5444972457694));
#11278=CARTESIAN_POINT('Ctrl Pts',(-2.21516439938128,-1.05098448937841,
92.5487213937602));
#11279=CARTESIAN_POINT('Ctrl Pts',(-2.17911472678708,-1.12383950280866,
92.552945541751));
#11280=CARTESIAN_POINT('Ctrl Pts',(-2.13948608332324,-1.19480105007744,
92.5571696897417));
#11281=CARTESIAN_POINT('Ctrl Pts',(-2.09965263892713,-1.26612932680668,
92.5614156681403));
#11282=CARTESIAN_POINT('Ctrl Pts',(-2.05620326646652,-1.33554405505853,
92.5656616465388));
#11283=CARTESIAN_POINT('Ctrl Pts',(-2.00935211029651,-1.4026597402246,92.5699076249373));
#11284=CARTESIAN_POINT('Ctrl Pts',(-1.96282619586518,-1.46930950685375,
92.5741241276621));
#11285=CARTESIAN_POINT('Ctrl Pts',(-1.91294584845879,-1.53369166287166,
92.5783406303868));
#11286=CARTESIAN_POINT('Ctrl Pts',(-1.8599655640961,-1.59545553067977,92.5825571331115));
#11287=CARTESIAN_POINT('Ctrl Pts',(-1.80700290805457,-1.65719884757331,
92.5867722328641));
#11288=CARTESIAN_POINT('Ctrl Pts',(-1.7509426659481,-1.71632525347441,92.5909873326167));
#11289=CARTESIAN_POINT('Ctrl Pts',(-1.69207977436681,-1.77251693565358,
92.5952024323692));
#11290=CARTESIAN_POINT('Ctrl Pts',(-1.63321841129507,-1.82870715868726,
92.5994174226671));
#11291=CARTESIAN_POINT('Ctrl Pts',(-1.57155488066292,-1.88196248907348,
92.603632412965));
#11292=CARTESIAN_POINT('Ctrl Pts',(-1.50742010717977,-1.93200281326662,
92.6078474032628));
#11293=CARTESIAN_POINT('Ctrl Pts',(-1.4424663588154,-1.9826821319761,92.6121162172665));
#11294=CARTESIAN_POINT('Ctrl Pts',(-1.37497818012107,-2.03006343782352,
92.6163850312701));
#11295=CARTESIAN_POINT('Ctrl Pts',(-1.30533134409059,-2.07389978835397,
92.6206538452738));
#11296=CARTESIAN_POINT('Ctrl Pts',(-1.23646235739739,-2.11724655345381,
92.624874983111));
#11297=CARTESIAN_POINT('Ctrl Pts',(-1.16548313209144,-2.15712697598517,
92.6290961209483));
#11298=CARTESIAN_POINT('Ctrl Pts',(-1.09278190898211,-2.19334856997273,
92.6333172587855));
#11299=CARTESIAN_POINT('Ctrl Pts',(-1.01884898636047,-2.230183827909,92.6376099108724));
#11300=CARTESIAN_POINT('Ctrl Pts',(-0.943135637492417,-2.2632349308766,
92.6419025629592));
#11301=CARTESIAN_POINT('Ctrl Pts',(-0.866069566338952,-2.29235114157091,
92.6461952150461));
#11302=CARTESIAN_POINT('Ctrl Pts',(-0.789003495185486,-2.32146735226522,
92.6504878671329));
#11303=CARTESIAN_POINT('Ctrl Pts',(-0.710585196862659,-2.34664858167637,
92.6547805192198));
#11304=CARTESIAN_POINT('Ctrl Pts',(-0.631254648110631,-2.36779809511679,
92.6590731713066));
#11305=CARTESIAN_POINT('Ctrl Pts',(-0.553077606236169,-2.38864008378152,
92.6633034060299));
#11306=CARTESIAN_POINT('Ctrl Pts',(-0.473719831384154,-2.40564548227121,
92.6675336407531));
#11307=CARTESIAN_POINT('Ctrl Pts',(-0.393592456264391,-2.41868460704817,
92.6717638754764));
#11308=CARTESIAN_POINT('Ctrl Pts',(-0.31358040377632,-2.43170496537756,
92.6759880218709));
#11309=CARTESIAN_POINT('Ctrl Pts',(-0.232801406065574,-2.44077031305807,
92.6802121682654));
#11310=CARTESIAN_POINT('Ctrl Pts',(-0.151680162123258,-2.44580117311654,
92.68443631466));
#11311=CARTESIAN_POINT('Ctrl Pts',(-0.0701396449149185,-2.45085803505844,
92.688682293457));
#11312=CARTESIAN_POINT('Ctrl Pts',(0.0117462071124492,-2.45183845801596,
92.6929282722542));
#11313=CARTESIAN_POINT('Ctrl Pts',(0.0935373210967758,-2.44871415636085,
92.6971742510512));
#11314=CARTESIAN_POINT('Ctrl Pts',(0.174760601070809,-2.44561154513948,
92.701390752182));
#11315=CARTESIAN_POINT('Ctrl Pts',(0.25588998330297,-2.43846104083498,92.7056072533127));
#11316=CARTESIAN_POINT('Ctrl Pts',(0.336492867185838,-2.4272871277072,92.7098237544435));
#11317=CARTESIAN_POINT('Ctrl Pts',(0.417068931855568,-2.41611693250541,
92.7140388526065));
#11318=CARTESIAN_POINT('Ctrl Pts',(0.497118385644902,-2.40092605074118,
92.7182539507696));
#11319=CARTESIAN_POINT('Ctrl Pts',(0.576214409324468,-2.38179075581522,
92.7224690489326));
#11320=CARTESIAN_POINT('Ctrl Pts',(0.655308379219406,-2.36265595775084,
92.7266840376477));
#11321=CARTESIAN_POINT('Ctrl Pts',(0.733448516334295,-2.33957706057718,
92.7308990263627));
#11322=CARTESIAN_POINT('Ctrl Pts',(0.810220256939178,-2.31268099513215,
92.7351140150777));
#11323=CARTESIAN_POINT('Ctrl Pts',(0.887972404943038,-2.28544145562546,
92.7393828309704));
#11324=CARTESIAN_POINT('Ctrl Pts',(0.964320490939832,-2.25428670631132,
92.7436516468631));
#11325=CARTESIAN_POINT('Ctrl Pts',(1.03885360603746,-2.21939934108825,92.7479204627558));
#11326=CARTESIAN_POINT('Ctrl Pts',(1.1125542398088,-2.18490164266005,92.7521415990432));
#11327=CARTESIAN_POINT('Ctrl Pts',(1.18447985772426,-2.14675456991049,92.7563627353305));
#11328=CARTESIAN_POINT('Ctrl Pts',(1.25425862109093,-2.10518064816753,92.7605838716178));
#11329=CARTESIAN_POINT('Ctrl Pts',(1.32521965755015,-2.06290233261395,92.7648765273132));
#11330=CARTESIAN_POINT('Ctrl Pts',(1.39395999724159,-2.01708024633689,92.7691691830086));
#11331=CARTESIAN_POINT('Ctrl Pts',(1.46012158338997,-1.96799268589057,92.773461838704));
#11332=CARTESIAN_POINT('Ctrl Pts',(1.52628316953835,-1.91890512544425,92.7777544943994));
#11333=CARTESIAN_POINT('Ctrl Pts',(1.58986565956419,-1.86655245921086,92.7820471500948));
#11334=CARTESIAN_POINT('Ctrl Pts',(1.65054978974358,-1.81125250629983,92.7863398057902));
#11335=CARTESIAN_POINT('Ctrl Pts',(1.71035147192646,-1.75675670650938,92.7905700391454));
#11336=CARTESIAN_POINT('Ctrl Pts',(1.7675641112248,-1.69919327125266,92.7948002725007));
#11337=CARTESIAN_POINT('Ctrl Pts',(1.82185632257683,-1.63883793887219,92.7990305058559));
#11338=CARTESIAN_POINT('Ctrl Pts',(1.87607039392428,-1.57856947283646,92.8032546508525));
#11339=CARTESIAN_POINT('Ctrl Pts',(1.92737207662859,-1.5155174329386,92.807478795849));
#11340=CARTESIAN_POINT('Ctrl Pts',(1.97546488571195,-1.44999611562207,92.8117029408456));
#11341=CARTESIAN_POINT('Ctrl Pts',(2.02380628129709,-1.38413612573941,92.8159489199884));
#11342=CARTESIAN_POINT('Ctrl Pts',(2.06890517990798,-1.31578157587251,92.8201948991313));
#11343=CARTESIAN_POINT('Ctrl Pts',(2.11049984743144,-1.24528737405944,92.8244408782741));
#11344=CARTESIAN_POINT('Ctrl Pts',(2.1518057267086,-1.17528260750641,92.8286573779442));
#11345=CARTESIAN_POINT('Ctrl Pts',(2.18965564044924,-1.10316821168101,92.8328738776142));
#11346=CARTESIAN_POINT('Ctrl Pts',(2.2238362864575,-1.02932134002698,92.8370903772842));
#11347=CARTESIAN_POINT('Ctrl Pts',(2.2580055592786,-0.955499040006019,92.8413054739661));
#11348=CARTESIAN_POINT('Ctrl Pts',(2.28850779359906,-0.879945830712804,
92.8455205706481));
#11349=CARTESIAN_POINT('Ctrl Pts',(2.31517637954871,-0.803062003571175,
92.84973566733));
#11350=CARTESIAN_POINT('Ctrl Pts',(2.34184427291244,-0.72618017311041,92.8539506545454));
#11351=CARTESIAN_POINT('Ctrl Pts',(2.36467856441186,-0.647968233352739,
92.8581656417608));
#11352=CARTESIAN_POINT('Ctrl Pts',(2.38356188492226,-0.568843555598427,
92.8623806289763));
#11353=CARTESIAN_POINT('Ctrl Pts',(2.40268636786249,-0.488708361736159,
92.8666494465844));
#11354=CARTESIAN_POINT('Ctrl Pts',(2.41775811482212,-0.407637422049397,
92.8709182641925));
#11355=CARTESIAN_POINT('Ctrl Pts',(2.42870855794048,-0.326075130279298,
92.8751870818006));
#11356=CARTESIAN_POINT('Ctrl Pts',(2.43953668420367,-0.245423892328883,
92.879408216558));
#11357=CARTESIAN_POINT('Ctrl Pts',(2.44633514093541,-0.164292698917119,
92.8836293513154));
#11358=CARTESIAN_POINT('Ctrl Pts',(2.44909007639386,-0.0831146660291083,
92.8878504860727));
#11359=CARTESIAN_POINT('Ctrl Pts',(2.45189169237209,-0.000561126227321199,
92.8921431451062));
#11360=CARTESIAN_POINT('Ctrl Pts',(2.45051149473331,0.0820403524250221,
92.8964358041397));
#11361=CARTESIAN_POINT('Ctrl Pts',(2.44498999982381,0.164238091688756,92.9007284631733));
#11362=CARTESIAN_POINT('Ctrl Pts',(2.43946850491431,0.246435830952492,92.9050211222068));
#11363=CARTESIAN_POINT('Ctrl Pts',(2.42980583740192,0.328229343459863,92.9093137812403));
#11364=CARTESIAN_POINT('Ctrl Pts',(2.41609673601504,0.409178215717133,92.9136064402738));
#11365=CARTESIAN_POINT('Ctrl Pts',(2.40258699467626,0.488949915918327,92.9178366747408));
#11366=CARTESIAN_POINT('Ctrl Pts',(2.38509682483617,0.568202252882996,92.9220669092078));
#11367=CARTESIAN_POINT('Ctrl Pts',(2.36367901183605,0.64650736964536,92.9262971436748));
#11368=CARTESIAN_POINT('Ctrl Pts',(2.34229202430589,0.724699786197636,92.9305212898001));
#11369=CARTESIAN_POINT('Ctrl Pts',(2.3169887420444,0.801947245197778,92.9347454359253));
#11370=CARTESIAN_POINT('Ctrl Pts',(2.28787325634421,0.877830400991535,92.9389695820505));
#11371=CARTESIAN_POINT('Ctrl Pts',(2.25860728561363,0.954105763156957,92.9432155609133));
#11372=CARTESIAN_POINT('Ctrl Pts',(2.22548966609151,1.02900220793019,92.9474615397761));
#11373=CARTESIAN_POINT('Ctrl Pts',(2.18867744163181,1.10210766556268,92.9517075186389));
#11374=CARTESIAN_POINT('Ctrl Pts',(2.15212078884102,1.17470558299384,92.9559240194704));
#11375=CARTESIAN_POINT('Ctrl Pts',(2.11192088078324,1.24553688170727,92.9601405203019));
#11376=CARTESIAN_POINT('Ctrl Pts',(2.06827966112225,1.31421820615453,92.9643570211334));
#11377=CARTESIAN_POINT('Ctrl Pts',(2.02465296243216,1.38287667790607,92.9685721189866));
#11378=CARTESIAN_POINT('Ctrl Pts',(1.97758747525721,1.44938620366654,92.9727872168398));
#11379=CARTESIAN_POINT('Ctrl Pts',(1.92732985321778,1.51339019651098,92.9770023146929));
#11380=CARTESIAN_POINT('Ctrl Pts',(1.87707353627578,1.57739252729018,92.9812173030878));
#11381=CARTESIAN_POINT('Ctrl Pts',(1.82362553740962,1.63888908930236,92.9854322914827));
#11382=CARTESIAN_POINT('Ctrl Pts',(1.76727350183467,1.6975554835448,92.9896472798776));
#11383=CARTESIAN_POINT('Ctrl Pts',(1.71020181809974,1.75697108164897,92.9939160961176));
#11384=CARTESIAN_POINT('Ctrl Pts',(1.65015172398301,1.81348334779756,92.9981849123576));
#11385=CARTESIAN_POINT('Ctrl Pts',(1.58745998202576,1.86679432596812,93.0024537285975));
#11386=CARTESIAN_POINT('Ctrl Pts',(1.52546847183818,1.91950985026515,93.0066748645425));
#11387=CARTESIAN_POINT('Ctrl Pts',(1.46089444274103,1.96909500614548,93.0108960004875));
#11388=CARTESIAN_POINT('Ctrl Pts',(1.39409475467345,2.01530396342387,93.0151171364325));
#11389=CARTESIAN_POINT('Ctrl Pts',(1.32616325201592,2.0622958580714,93.01940979282));
#11390=CARTESIAN_POINT('Ctrl Pts',(1.25593039761607,2.10579581939649,93.0237024492075));
#11391=CARTESIAN_POINT('Ctrl Pts',(1.18379806120738,2.14559371743153,93.027995105595));
#11392=CARTESIAN_POINT('Ctrl Pts',(1.11166572479868,2.18539161546657,93.0322877619825));
#11393=CARTESIAN_POINT('Ctrl Pts',(1.03763438377147,2.22148729157579,93.03658041837));
#11394=CARTESIAN_POINT('Ctrl Pts',(0.962125748599477,2.25372231960415,93.0408730747575));
#11395=CARTESIAN_POINT('Ctrl Pts',(0.887715131358506,2.28548859808219,93.045103308964));
#11396=CARTESIAN_POINT('Ctrl Pts',(0.811589274561371,2.31362562066973,93.0493335431706));
#11397=CARTESIAN_POINT('Ctrl Pts',(0.734136643297586,2.33794645767771,93.0535637773772));
#11398=CARTESIAN_POINT('Ctrl Pts',(0.656795485347559,2.36223229104217,93.0577879232403));
#11399=CARTESIAN_POINT('Ctrl Pts',(0.578131785408882,2.38271270881352,93.0620120691033));
#11400=CARTESIAN_POINT('Ctrl Pts',(0.498554588782068,2.39924854319104,93.0662362149664));
#11401=CARTESIAN_POINT('Ctrl Pts',(0.418566086730034,2.41586984524873,93.0704821938945));
#11402=CARTESIAN_POINT('Ctrl Pts',(0.337655054348106,2.42850547916418,93.0747281728226));
#11403=CARTESIAN_POINT('Ctrl Pts',(0.256253046795857,2.43706475621963,93.0789741517507));
#11404=CARTESIAN_POINT('Ctrl Pts',(0.175416185187573,2.44556460917908,93.0831906523178));
#11405=CARTESIAN_POINT('Ctrl Pts',(0.094095612890168,2.45004447821745,93.0874071528849));
#11406=CARTESIAN_POINT('Ctrl Pts',(0.012723006264846,2.4504669708265,93.0916236534519));
#11407=CARTESIAN_POINT('Ctrl Pts',(-0.0686225248214064,2.45088932285733,
93.0958387510404));
#11408=CARTESIAN_POINT('Ctrl Pts',(-0.150019591046555,2.44725697694501,
93.1000538486288));
#11409=CARTESIAN_POINT('Ctrl Pts',(-0.231034860726386,2.43958462512149,
93.1042689462173));
#11410=CARTESIAN_POINT('Ctrl Pts',(-0.312048026591457,2.43191247253456,
93.1084839343476));
#11411=CARTESIAN_POINT('Ctrl Pts',(-0.392678952610482,2.420200567542,93.1126989224778));
#11412=CARTESIAN_POINT('Ctrl Pts',(-0.472499221088961,2.40451548883976,
93.1169139106081));
#11413=CARTESIAN_POINT('Ctrl Pts',(-0.553338851663316,2.38863010042917,
93.1211827271608));
#11414=CARTESIAN_POINT('Ctrl Pts',(-0.633346489175556,2.36866941352884,
93.1254515437136));
#11415=CARTESIAN_POINT('Ctrl Pts',(-0.712089403515037,2.3447556229598,93.1297203602664));
#11416=CARTESIAN_POINT('Ctrl Pts',(-0.789952792916594,2.32110893928339,
93.1339414959497));
#11417=CARTESIAN_POINT('Ctrl Pts',(-0.866579149086681,2.29359723875549,
93.1381626316331));
#11418=CARTESIAN_POINT('Ctrl Pts',(-0.941568725504837,2.26238780609143,
93.1423837673165));
#11419=CARTESIAN_POINT('Ctrl Pts',(-1.01782889654489,2.23064957277014,93.1466764243039));
#11420=CARTESIAN_POINT('Ctrl Pts',(-1.09239585355719,2.19508735535688,93.1509690812914));
#11421=CARTESIAN_POINT('Ctrl Pts',(-1.16487554585739,2.1559256046217,93.1552617382788));
#11422=CARTESIAN_POINT('Ctrl Pts',(-1.23735523815759,2.11676385388653,93.1595543952663));
#11423=CARTESIAN_POINT('Ctrl Pts',(-1.30774727418056,2.07400288565244,93.1638470522537));
#11424=CARTESIAN_POINT('Ctrl Pts',(-1.37569037043724,2.02791179657456,93.1681397092411));
#11425=CARTESIAN_POINT('Ctrl Pts',(-1.44236725713998,1.98267967596525,93.1723523668823));
#11426=CARTESIAN_POINT('Ctrl Pts',(-1.50694183239721,1.9340667131829,93.1765650245233));
#11427=CARTESIAN_POINT('Ctrl Pts',(-1.56904854747722,1.88229564778215,93.1807776821644));
#11428=CARTESIAN_POINT('Ctrl Pts',(-1.63106572752764,1.83059921720739,93.1849842667034));
#11429=CARTESIAN_POINT('Ctrl Pts',(-1.69062175416469,1.77575402204514,93.1891908512423));
#11430=CARTESIAN_POINT('Ctrl Pts',(-1.74737996150074,1.71802605339549,93.1933974357812));
#11431=CARTESIAN_POINT('Ctrl Pts',(-1.80407245956903,1.66036491671123,93.1975991503356));
#11432=CARTESIAN_POINT('Ctrl Pts',(-1.85797324684742,1.59982797090653,93.2018008648901));
#11433=CARTESIAN_POINT('Ctrl Pts',(-1.90877985805194,1.5367204376513,93.2060025794445));
#11434=CARTESIAN_POINT('Ctrl Pts',(-1.95955446527867,1.47365265694098,93.210201647265));
#11435=CARTESIAN_POINT('Ctrl Pts',(-2.00723847084698,1.40801786702482,93.2144007150856));
#11436=CARTESIAN_POINT('Ctrl Pts',(-2.05156816015713,1.34015608577116,93.2185997829061));
#11437=CARTESIAN_POINT('Ctrl Pts',(-2.09588382052396,1.27231578062297,93.2227975218546));
#11438=CARTESIAN_POINT('Ctrl Pts',(-2.13684701574996,1.20225027628605,93.2269952608031));
#11439=CARTESIAN_POINT('Ctrl Pts',(-2.17423691200447,1.13032920004628,93.2311929997516));
#11440=CARTESIAN_POINT('Ctrl Pts',(-2.21162669527163,1.05840834114253,93.2353907260151));
#11441=CARTESIAN_POINT('Ctrl Pts',(-2.24544298590763,0.984632338829554,
93.2395884522786));
#11442=CARTESIAN_POINT('Ctrl Pts',(-2.27551124887344,0.909394747208525,
93.2437861785421));
#11443=CARTESIAN_POINT('Ctrl Pts',(-2.30560923408867,0.83408278379999,93.2479880542261));
#11444=CARTESIAN_POINT('Ctrl Pts',(-2.33195161769914,0.757306782595229,
93.2521899299101));
#11445=CARTESIAN_POINT('Ctrl Pts',(-2.35441257145108,0.679478986719307,
93.2563918055941));
#11446=CARTESIAN_POINT('Ctrl Pts',(-2.37688462206551,0.601612739922845,
93.2605957572201));
#11447=CARTESIAN_POINT('Ctrl Pts',(-2.39547131671404,0.52269412116537,93.264799708846));
#11448=CARTESIAN_POINT('Ctrl Pts',(-2.41009776619079,0.443146710923332,
93.269003660472));
#11449=CARTESIAN_POINT('Ctrl Pts',(-2.42475001582833,0.363458983923097,
93.2732150276111));
#11450=CARTESIAN_POINT('Ctrl Pts',(-2.43542800427714,0.283140716005997,
93.2774263947502));
#11451=CARTESIAN_POINT('Ctrl Pts',(-2.44210867626308,0.202621477935082,
93.2816377618892));
#11452=CARTESIAN_POINT('Ctrl Pts',(-2.44771819378852,0.13501239938064,93.2851738938566));
#11453=CARTESIAN_POINT('Ctrl Pts',(-2.4505103917333,0.0672618352071985,
93.2887100258239));
#11454=CARTESIAN_POINT('Ctrl Pts',(-2.45049997091768,-0.00037753468746127,
93.2922461577912));
#11455=CARTESIAN_POINT('',(-2.45049896913575,0.00224772432606832,94.0922461578025));
#11456=CARTESIAN_POINT('Ctrl Pts',(-2.45049997091754,-0.000377535622314954,
93.2922461578401));
#11457=CARTESIAN_POINT('Ctrl Pts',(-2.45049686660316,-0.020526951609039,
93.293299553135));
#11458=CARTESIAN_POINT('Ctrl Pts',(-2.45024524718698,-0.0406742062679038,
93.2943529484299));
#11459=CARTESIAN_POINT('Ctrl Pts',(-2.44974524247741,-0.0608152691294603,
93.2954063437248));
#11460=CARTESIAN_POINT('Ctrl Pts',(-2.44773731911088,-0.141697928777799,
93.2996365779332));
#11461=CARTESIAN_POINT('Ctrl Pts',(-2.44171557726676,-0.22263356198852,
93.3038668121415));
#11462=CARTESIAN_POINT('Ctrl Pts',(-2.43167131269257,-0.303191155919789,
93.3080970463499));
#11463=CARTESIAN_POINT('Ctrl Pts',(-2.42164150427865,-0.383632807715177,
93.3123211922137));
#11464=CARTESIAN_POINT('Ctrl Pts',(-2.40760072815549,-0.46369704314202,
93.3165453380776));
#11465=CARTESIAN_POINT('Ctrl Pts',(-2.38959227524804,-0.542953964968405,
93.3207694839414));
#11466=CARTESIAN_POINT('Ctrl Pts',(-2.37149074323843,-0.622620536816421,
93.3250154628692));
#11467=CARTESIAN_POINT('Ctrl Pts',(-2.34938040888767,-0.701470949068802,
93.329261441797));
#11468=CARTESIAN_POINT('Ctrl Pts',(-2.32335801214661,-0.779074962628212,
93.3335074207248));
#11469=CARTESIAN_POINT('Ctrl Pts',(-2.29751627990227,-0.856140198372773,
93.33772392129));
#11470=CARTESIAN_POINT('Ctrl Pts',(-2.26781678328248,-0.931975840389033,
93.3419404218552));
#11471=CARTESIAN_POINT('Ctrl Pts',(-2.23440479463291,-1.00617367473089,
93.3461569224204));
#11472=CARTESIAN_POINT('Ctrl Pts',(-2.20100392333932,-1.08034682081651,
93.350372020006));
#11473=CARTESIAN_POINT('Ctrl Pts',(-2.16389320388801,-1.1528828175805,93.3545871175917));
#11474=CARTESIAN_POINT('Ctrl Pts',(-2.12326597596168,-1.22339357744084,
93.3588022151773));
#11475=CARTESIAN_POINT('Ctrl Pts',(-2.08263980305785,-1.29390250625235,
93.3630172033038));
#11476=CARTESIAN_POINT('Ctrl Pts',(-2.03849753640268,-1.36238590019093,
93.3672321914303));
#11477=CARTESIAN_POINT('Ctrl Pts',(-1.9910776745944,-1.42848169177338,93.3714471795567));
#11478=CARTESIAN_POINT('Ctrl Pts',(-1.94305222706854,-1.49542157411968,
93.375715996111));
#11479=CARTESIAN_POINT('Ctrl Pts',(-1.89166514559194,-1.55991203050682,
93.3799848126653));
#11480=CARTESIAN_POINT('Ctrl Pts',(-1.83720731224929,-1.6216101694975,93.3842536292196));
#11481=CARTESIAN_POINT('Ctrl Pts',(-1.78335774989377,-1.68261916634639,
93.3884747648968));
#11482=CARTESIAN_POINT('Ctrl Pts',(-1.72650606536615,-1.74089761948361,
93.392695900574));
#11483=CARTESIAN_POINT('Ctrl Pts',(-1.66697045874657,-1.79615136880671,
93.3969170362512));
#11484=CARTESIAN_POINT('Ctrl Pts',(-1.60642610347734,-1.85234131661981,
93.4012096932441));
#11485=CARTESIAN_POINT('Ctrl Pts',(-1.54310641699523,-1.90540278796908,
93.4055023502369));
#11486=CARTESIAN_POINT('Ctrl Pts',(-1.4773792360893,-1.95507054675073,93.4097950072298));
#11487=CARTESIAN_POINT('Ctrl Pts',(-1.41165205518336,-2.00473830553238,
93.4140876642226));
#11488=CARTESIAN_POINT('Ctrl Pts',(-1.34351782977679,-2.05101212672075,
93.4183803212155));
#11489=CARTESIAN_POINT('Ctrl Pts',(-1.27337140062822,-2.09367512428794,
93.4226729782083));
#11490=CARTESIAN_POINT('Ctrl Pts',(-1.20424502459612,-2.13571772643152,
93.426903212378));
#11491=CARTESIAN_POINT('Ctrl Pts',(-1.13290389007825,-2.1744124353288,93.4311334465477));
#11492=CARTESIAN_POINT('Ctrl Pts',(-1.05970587076521,-2.20951888823467,
93.4353636807174));
#11493=CARTESIAN_POINT('Ctrl Pts',(-0.986613201362138,-2.24457481434092,
93.4395878265421));
#11494=CARTESIAN_POINT('Ctrl Pts',(-0.91166937073539,-2.27605254165549,
93.4438119723669));
#11495=CARTESIAN_POINT('Ctrl Pts',(-0.835259426902683,-2.30375605040338,
93.4480361181917));
#11496=CARTESIAN_POINT('Ctrl Pts',(-0.758454547149536,-2.33160274877004,
93.4522820971292));
#11497=CARTESIAN_POINT('Ctrl Pts',(-0.680168759841889,-2.35563584966458,
93.4565280760667));
#11498=CARTESIAN_POINT('Ctrl Pts',(-0.600816299475869,-2.37570411126557,
93.4607740550042));
#11499=CARTESIAN_POINT('Ctrl Pts',(-0.522014756707144,-2.39563304563698,
93.4649905555298));
#11500=CARTESIAN_POINT('Ctrl Pts',(-0.442161762012838,-2.41165190392492,
93.4692070560554));
#11501=CARTESIAN_POINT('Ctrl Pts',(-0.361679262256269,-2.42366217968878,
93.473423556581));
#11502=CARTESIAN_POINT('Ctrl Pts',(-0.281223541890074,-2.43566845920669,
93.4776386541268));
#11503=CARTESIAN_POINT('Ctrl Pts',(-0.200139192128692,-2.44366873625792,
93.4818537516727));
#11504=CARTESIAN_POINT('Ctrl Pts',(-0.118857218081033,-2.44761582191937,
93.4860688492186));
#11505=CARTESIAN_POINT('Ctrl Pts',(-0.0375773547942155,-2.45156280508142,
93.4902838373053));
#11506=CARTESIAN_POINT('Ctrl Pts',(0.0438996578856404,-2.45145678462448,
93.4944988253919));
#11507=CARTESIAN_POINT('Ctrl Pts',(0.125140287105287,-2.4473026291293,93.4987138134786));
#11508=CARTESIAN_POINT('Ctrl Pts',(0.207418419230373,-2.44309542199682,
93.5029826300797));
#11509=CARTESIAN_POINT('Ctrl Pts',(0.28945359834815,-2.43473595704496,93.5072514466808));
#11510=CARTESIAN_POINT('Ctrl Pts',(0.370800100238823,-2.42228353742143,
93.5115202632819));
#11511=CARTESIAN_POINT('Ctrl Pts',(0.451237994439687,-2.40997020631386,
93.5157413989195));
#11512=CARTESIAN_POINT('Ctrl Pts',(0.531002070396874,-2.39365505375892,
93.5199625345571));
#11513=CARTESIAN_POINT('Ctrl Pts',(0.609672827741539,-2.37344671166505,
93.5241836701947));
#11514=CARTESIAN_POINT('Ctrl Pts',(0.689676554872338,-2.35289596649349,
93.5284763272776));
#11515=CARTESIAN_POINT('Ctrl Pts',(0.768549090080892,-2.32831902775211,
93.5327689843605));
#11516=CARTESIAN_POINT('Ctrl Pts',(0.845868426999605,-2.29988192179625,
93.5370616414434));
#11517=CARTESIAN_POINT('Ctrl Pts',(0.923187763918315,-2.27144481584039,
93.5413542985263));
#11518=CARTESIAN_POINT('Ctrl Pts',(0.998953469984371,-2.23914779949084,
93.5456469556092));
#11519=CARTESIAN_POINT('Ctrl Pts',(1.07276961171991,-2.20320575756562,93.5499396126921));
#11520=CARTESIAN_POINT('Ctrl Pts',(1.1455123345218,-2.16778637731588,93.5541698468512));
#11521=CARTESIAN_POINT('Ctrl Pts',(1.2166361949348,-2.12869373847066,93.5584000810103));
#11522=CARTESIAN_POINT('Ctrl Pts',(1.28574549763879,-2.08609893468684,93.5626303151694));
#11523=CARTESIAN_POINT('Ctrl Pts',(1.3547553350938,-2.04356543528027,93.5668544609833));
#11524=CARTESIAN_POINT('Ctrl Pts',(1.42175598060787,-1.99754002349982,93.5710786067972));
#11525=CARTESIAN_POINT('Ctrl Pts',(1.48637434874918,-1.9482406282029,93.5753027526111));
#11526=CARTESIAN_POINT('Ctrl Pts',(1.55132670654323,-1.89868642164429,93.5795487315513));
#11527=CARTESIAN_POINT('Ctrl Pts',(1.61387165934902,-1.84582449470403,93.5837947104914));
#11528=CARTESIAN_POINT('Ctrl Pts',(1.67365800960765,-1.78992153930729,93.5880406894316));
#11529=CARTESIAN_POINT('Ctrl Pts',(1.73302928302839,-1.73440669962348,93.5922571899457));
#11530=CARTESIAN_POINT('Ctrl Pts',(1.78967979246899,-1.67589324537274,93.5964736904597));
#11531=CARTESIAN_POINT('Ctrl Pts',(1.84329853290387,-1.61468286935684,93.6006901909737));
#11532=CARTESIAN_POINT('Ctrl Pts',(1.89689943247359,-1.55349286021372,93.6049052885078));
#11533=CARTESIAN_POINT('Ctrl Pts',(1.94747025999694,-1.48960806092931,93.6091203860419));
#11534=CARTESIAN_POINT('Ctrl Pts',(1.99473828254142,-1.42336553076281,93.6133354835759));
#11535=CARTESIAN_POINT('Ctrl Pts',(2.04200507760965,-1.35712472081071,93.6175504716505));
#11536=CARTESIAN_POINT('Ctrl Pts',(2.08596896889155,-1.2885266809942,93.6217654597252));
#11537=CARTESIAN_POINT('Ctrl Pts',(2.12639964896309,-1.21793874348821,93.6259804477998));
#11538=CARTESIAN_POINT('Ctrl Pts',(2.16734665896066,-1.1464493453962,93.6302492644144));
#11539=CARTESIAN_POINT('Ctrl Pts',(2.20466931471134,-1.07291927885784,93.6345180810291));
#11540=CARTESIAN_POINT('Ctrl Pts',(2.23817650900993,-0.997755563510491,
93.6387868976437));
#11541=CARTESIAN_POINT('Ctrl Pts',(2.27130944122984,-0.923431397070061,
93.6430080332689));
#11542=CARTESIAN_POINT('Ctrl Pts',(2.30071160980411,-0.847510356062231,
93.647229168894));
#11543=CARTESIAN_POINT('Ctrl Pts',(2.32624758298905,-0.770404071015732,
93.6514503045192));
#11544=CARTESIAN_POINT('Ctrl Pts',(2.35221622900574,-0.691991323338812,
93.6557429616286));
#11545=CARTESIAN_POINT('Ctrl Pts',(2.37418631550918,-0.612353278914442,
93.660035618738));
#11546=CARTESIAN_POINT('Ctrl Pts',(2.39206933760362,-0.531934708490236,
93.6643282758474));
#11547=CARTESIAN_POINT('Ctrl Pts',(2.40995235969806,-0.451516138066032,
93.6686209329568));
#11548=CARTESIAN_POINT('Ctrl Pts',(2.42374829954972,-0.370317544383954,
93.6729135900662));
#11549=CARTESIAN_POINT('Ctrl Pts',(2.43342385047315,-0.288788181801841,
93.6772062471756));
#11550=CARTESIAN_POINT('Ctrl Pts',(2.44295870152505,-0.208444402442073,
93.6814364813482));
#11551=CARTESIAN_POINT('Ctrl Pts',(2.44852821755694,-0.127476393511042,
93.6856667155208));
#11552=CARTESIAN_POINT('Ctrl Pts',(2.45006238231793,-0.0463095319623845,
93.6898969496934));
#11553=CARTESIAN_POINT('Ctrl Pts',(2.45159433903938,0.0347405105559447,
93.694121095521));
#11554=CARTESIAN_POINT('Ctrl Pts',(2.44910247039975,0.115988376156796,93.6983452413487));
#11555=CARTESIAN_POINT('Ctrl Pts',(2.44256838395305,0.19700238504394,93.7025693871763));
#11556=CARTESIAN_POINT('Ctrl Pts',(2.43600052513471,0.278435126563032,93.7068153661131));
#11557=CARTESIAN_POINT('Ctrl Pts',(2.42534848213189,0.359631114209472,93.7110613450499));
#11558=CARTESIAN_POINT('Ctrl Pts',(2.41064671769813,0.440150715609106,93.7153073239867));
#11559=CARTESIAN_POINT('Ctrl Pts',(2.39604702268683,0.520111296406298,93.7195238245149));
#11560=CARTESIAN_POINT('Ctrl Pts',(2.37745374454511,0.599404389413137,93.7237403250432));
#11561=CARTESIAN_POINT('Ctrl Pts',(2.35495252107438,0.677605249009643,93.7279568255715));
#11562=CARTESIAN_POINT('Ctrl Pts',(2.33245878456142,0.755780088397308,93.73217192312));
#11563=CARTESIAN_POINT('Ctrl Pts',(2.30605981341392,0.832862969375039,93.7363870206685));
#11564=CARTESIAN_POINT('Ctrl Pts',(2.2758916896718,0.908442219892288,93.740602118217));
#11565=CARTESIAN_POINT('Ctrl Pts',(2.2457243493474,0.984019507737804,93.7448171063062));
#11566=CARTESIAN_POINT('Ctrl Pts',(2.21178822447472,1.05809281111239,93.7490320943954));
#11567=CARTESIAN_POINT('Ctrl Pts',(2.17426780217715,1.13026977948441,93.7532470824846));
#11568=CARTESIAN_POINT('Ctrl Pts',(2.13626821639556,1.20336850101147,93.7575158990825));
#11569=CARTESIAN_POINT('Ctrl Pts',(2.09459234416314,1.27452166630813,93.7617847156803));
#11570=CARTESIAN_POINT('Ctrl Pts',(2.04947925360533,1.3433484428998,93.7660535322782));
#11571=CARTESIAN_POINT('Ctrl Pts',(2.00487005805567,1.4114064521842,93.7702746679182));
#11572=CARTESIAN_POINT('Ctrl Pts',(1.95690037414002,1.47718943973062,93.7744958035581));
#11573=CARTESIAN_POINT('Ctrl Pts',(1.90584325146648,1.54036091577256,93.778716939198));
#11574=CARTESIAN_POINT('Ctrl Pts',(1.85392103487245,1.60460274707563,93.7830095962749));
#11575=CARTESIAN_POINT('Ctrl Pts',(1.79880611936775,1.66614337431273,93.7873022533518));
#11576=CARTESIAN_POINT('Ctrl Pts',(1.74082480547681,1.72466786560097,93.7915949104286));
#11577=CARTESIAN_POINT('Ctrl Pts',(1.68284349158587,1.78319235688922,93.7958875675055));
#11578=CARTESIAN_POINT('Ctrl Pts',(1.62199619258673,1.8387004254033,93.8001802245824));
#11579=CARTESIAN_POINT('Ctrl Pts',(1.5586428253669,1.89092114931646,93.8044728816592));
#11580=CARTESIAN_POINT('Ctrl Pts',(1.49621072937485,1.94238249053939,93.8087031158274));
#11581=CARTESIAN_POINT('Ctrl Pts',(1.4311095326108,1.99084559138337,93.8129333499956));
#11582=CARTESIAN_POINT('Ctrl Pts',(1.36365921747145,2.03602155897357,93.8171635841638));
#11583=CARTESIAN_POINT('Ctrl Pts',(1.29630597988765,2.08113250726038,93.821387729987));
#11584=CARTESIAN_POINT('Ctrl Pts',(1.22661072184333,2.12296546155753,93.8256118758102));
#11585=CARTESIAN_POINT('Ctrl Pts',(1.15492663987504,2.16127154853502,93.8298360216333));
#11586=CARTESIAN_POINT('Ctrl Pts',(1.08287204825753,2.19977562611878,93.8340820005712));
#11587=CARTESIAN_POINT('Ctrl Pts',(1.00880837945504,2.23471596665707,93.8383279795091));
#11588=CARTESIAN_POINT('Ctrl Pts',(0.933124097740295,2.26588386026653,93.842573958447));
#11589=CARTESIAN_POINT('Ctrl Pts',(0.857965266726225,2.2968353655961,93.8467904589706));
#11590=CARTESIAN_POINT('Ctrl Pts',(0.781208690093167,2.32406646032518,93.8510069594943));
#11591=CARTESIAN_POINT('Ctrl Pts',(0.70325797834281,2.34741953342328,93.855223460018));
#11592=CARTESIAN_POINT('Ctrl Pts',(0.625333203569053,2.37076483612267,93.8594385575618));
#11593=CARTESIAN_POINT('Ctrl Pts',(0.546215527961278,2.39023454618982,93.8636536551056));
#11594=CARTESIAN_POINT('Ctrl Pts',(0.466324838418034,2.40572055631455,93.8678687526495));
#11595=CARTESIAN_POINT('Ctrl Pts',(0.386436223508429,2.42120616429233,93.872083740734));
#11596=CARTESIAN_POINT('Ctrl Pts',(0.305775091462451,2.43270819053178,93.8762987288184));
#11597=CARTESIAN_POINT('Ctrl Pts',(0.224771247095008,2.44016969419738,93.8805137169029));
#11598=CARTESIAN_POINT('Ctrl Pts',(0.142732923655423,2.4477264867897,93.8847825335063));
#11599=CARTESIAN_POINT('Ctrl Pts',(0.0603435574257589,2.45113876008916,
93.8890513501096));
#11600=CARTESIAN_POINT('Ctrl Pts',(-0.0219472251692508,2.45040171590443,
93.8933201667129));
#11601=CARTESIAN_POINT('Ctrl Pts',(-0.103318852750464,2.44967290420742,
93.8975413023481));
#11602=CARTESIAN_POINT('Ctrl Pts',(-0.184593621574171,2.44488709555706,
93.9017624379833));
#11603=CARTESIAN_POINT('Ctrl Pts',(-0.265340834386893,2.43609205318823,
93.9059835736184));
#11604=CARTESIAN_POINT('Ctrl Pts',(-0.347456199853924,2.42714799068432,
93.9102762307058));
#11605=CARTESIAN_POINT('Ctrl Pts',(-0.429025469614802,2.41405765161002,
93.9145688877933));
#11606=CARTESIAN_POINT('Ctrl Pts',(-0.509607289736811,2.39692525128488,
93.9188615448807));
#11607=CARTESIAN_POINT('Ctrl Pts',(-0.590189109858818,2.37979285095975,
93.9231542019681));
#11608=CARTESIAN_POINT('Ctrl Pts',(-0.669783015604948,2.35861858196367,
93.9274468590555));
#11609=CARTESIAN_POINT('Ctrl Pts',(-0.747966499788094,2.3335587340358,93.9317395161429));
#11610=CARTESIAN_POINT('Ctrl Pts',(-0.825013056225563,2.30886330113379,
93.9359697503158));
#11611=CARTESIAN_POINT('Ctrl Pts',(-0.900980542187783,2.28030145499961,
93.9401999844887));
#11612=CARTESIAN_POINT('Ctrl Pts',(-0.975452924571176,2.24798617476744,
93.9444302186617));
#11613=CARTESIAN_POINT('Ctrl Pts',(-1.04981812292117,2.21571740415353,93.9486543644896));
#11614=CARTESIAN_POINT('Ctrl Pts',(-1.12269206818594,2.17970611183101,93.9528785103175));
#11615=CARTESIAN_POINT('Ctrl Pts',(-1.1936744345533,2.14011485539769,93.9571026561454));
#11616=CARTESIAN_POINT('Ctrl Pts',(-1.26502368355035,2.10031896582777,93.9613486350821));
#11617=CARTESIAN_POINT('Ctrl Pts',(-1.33446128837698,2.0569061397908,93.9655946140188));
#11618=CARTESIAN_POINT('Ctrl Pts',(-1.40160164122745,2.01009031869429,93.9698405929555));
#11619=CARTESIAN_POINT('Ctrl Pts',(-1.46827586111603,1.96359952414925,93.9740570934839));
#11620=CARTESIAN_POINT('Ctrl Pts',(-1.53268423950821,1.91375310619271,93.9782735940122));
#11621=CARTESIAN_POINT('Ctrl Pts',(-1.59447596508579,1.86080537584234,93.9824900945406));
#11622=CARTESIAN_POINT('Ctrl Pts',(-1.65624713035636,1.8078752630869,93.9867051920891));
#11623=CARTESIAN_POINT('Ctrl Pts',(-1.71540301879969,1.75184618956455,93.9909202896377));
#11624=CARTESIAN_POINT('Ctrl Pts',(-1.77162566265668,1.69301292417284,93.9951353871862));
#11625=CARTESIAN_POINT('Ctrl Pts',(-1.82784684650103,1.63418118658747,93.9993503752753));
#11626=CARTESIAN_POINT('Ctrl Pts',(-1.88113461658577,1.57254573896462,94.0035653633645));
#11627=CARTESIAN_POINT('Ctrl Pts',(-1.93120868537594,1.50843735817187,94.0077803514536));
#11628=CARTESIAN_POINT('Ctrl Pts',(-1.98192223697967,1.44351026604385,94.0120491680514));
#11629=CARTESIAN_POINT('Ctrl Pts',(-2.02933910651463,1.3760470038798,94.0163179846491));
#11630=CARTESIAN_POINT('Ctrl Pts',(-2.07321215311288,1.30642321557184,94.0205868012468));
#11631=CARTESIAN_POINT('Ctrl Pts',(-2.11659515549269,1.23757709687134,94.0248079368866));
#11632=CARTESIAN_POINT('Ctrl Pts',(-2.15651293011166,1.16661891696603,94.0290290725263));
#11633=CARTESIAN_POINT('Ctrl Pts',(-2.19277278687027,1.09393681497661,94.033250208166));
#11634=CARTESIAN_POINT('Ctrl Pts',(-2.22964701788347,1.02002321302489,94.0375428652427));
#11635=CARTESIAN_POINT('Ctrl Pts',(-2.26273802276296,0.944327188629773,
94.0418355223195));
#11636=CARTESIAN_POINT('Ctrl Pts',(-2.29189483860102,0.867276368174531,
94.0461281793963));
#11637=CARTESIAN_POINT('Ctrl Pts',(-2.32105165443908,0.790225547719291,
94.050420836473));
#11638=CARTESIAN_POINT('Ctrl Pts',(-2.34627419196474,0.71182042627785,94.0547134935498));
#11639=CARTESIAN_POINT('Ctrl Pts',(-2.36746548479031,0.632500931482782,
94.0590061506265));
#11640=CARTESIAN_POINT('Ctrl Pts',(-2.39481446363939,0.530133076754626,
94.0645461518225));
#11641=CARTESIAN_POINT('Ctrl Pts',(-2.41553687113253,0.425925319477767,
94.0700861530185));
#11642=CARTESIAN_POINT('Ctrl Pts',(-2.4294335776465,0.320628666534577,94.0756261542145));
#11643=CARTESIAN_POINT('Ctrl Pts',(-2.44333028416046,0.215332013591387,
94.0811661554105));
#11644=CARTESIAN_POINT('Ctrl Pts',(-2.45040109986711,0.108946103270164,
94.0867061566065));
#11645=CARTESIAN_POINT('Ctrl Pts',(-2.45049896913575,0.00224772432606995,
94.0922461578025));
#11646=CARTESIAN_POINT('',(-2.45049991819808,-0.000633175507849021,94.8922461578706));
#11647=CARTESIAN_POINT('Ctrl Pts',(-2.45049896913641,0.00224772360119427,
94.0922461578402));
#11648=CARTESIAN_POINT('Ctrl Pts',(-2.45057271168345,-0.0781474083459136,
94.0964204398822));
#11649=CARTESIAN_POINT('Ctrl Pts',(-2.44668583696763,-0.158638087010778,
94.1005947219241));
#11650=CARTESIAN_POINT('Ctrl Pts',(-2.43883687232859,-0.238798995329727,
94.1047690039661));
#11651=CARTESIAN_POINT('Ctrl Pts',(-2.43099234738414,-0.318914561368906,
94.1089409248639));
#11652=CARTESIAN_POINT('Ctrl Pts',(-2.41919022501533,-0.398700254556573,
94.1131128457616));
#11653=CARTESIAN_POINT('Ctrl Pts',(-2.40348106258373,-0.477733222417452,
94.1172847666594));
#11654=CARTESIAN_POINT('Ctrl Pts',(-2.38777572169291,-0.556746964064932,
94.1214556726612));
#11655=CARTESIAN_POINT('Ctrl Pts',(-2.3681653205176,-0.635007877358875,
94.125626578663));
#11656=CARTESIAN_POINT('Ctrl Pts',(-2.34475172025415,-0.712102254149771,
94.1297974846647));
#11657=CARTESIAN_POINT('Ctrl Pts',(-2.32133626790918,-0.789202729322328,
94.1339687205969));
#11658=CARTESIAN_POINT('Ctrl Pts',(-2.29411715983875,-0.865136030139195,
94.1381399565291));
#11659=CARTESIAN_POINT('Ctrl Pts',(-2.26324595694186,-0.939504118344522,
94.1423111924612));
#11660=CARTESIAN_POINT('Ctrl Pts',(-2.23234250510913,-1.01394989356819,
94.146486785785));
#11661=CARTESIAN_POINT('Ctrl Pts',(-2.19777952781821,-1.0868267529397,94.1506623791087));
#11662=CARTESIAN_POINT('Ctrl Pts',(-2.15975623063707,-1.15775786511013,
94.1548379724325));
#11663=CARTESIAN_POINT('Ctrl Pts',(-2.12171076230802,-1.22873033677055,
94.1590160005187));
#11664=CARTESIAN_POINT('Ctrl Pts',(-2.08020120611368,-1.29775439710323,
94.1631940286049));
#11665=CARTESIAN_POINT('Ctrl Pts',(-2.03547076110762,-1.36448123133884,
94.1673720566911));
#11666=CARTESIAN_POINT('Ctrl Pts',(-1.99066531938294,-1.43131994225288,
94.1715570898138));
#11667=CARTESIAN_POINT('Ctrl Pts',(-1.94262849669932,-1.49585336034432,
94.1757421229364));
#11668=CARTESIAN_POINT('Ctrl Pts',(-1.89164409947937,-1.55776533884436,
94.1799271560591));
#11669=CARTESIAN_POINT('Ctrl Pts',(-1.86587544065273,-1.58905704254671,
94.1820423657428));
#11670=CARTESIAN_POINT('Ctrl Pts',(-1.83935441286635,-1.61967967395596,
94.1841575754264));
#11671=CARTESIAN_POINT('Ctrl Pts',(-1.81212105752399,-1.64959616963612,
94.1862727851101));
#11672=CARTESIAN_POINT('Ctrl Pts',(-1.75765673124764,-1.7094265416665,94.1905030192809));
#11673=CARTESIAN_POINT('Ctrl Pts',(-1.70012340622187,-1.76666948427848,
94.1947332534517));
#11674=CARTESIAN_POINT('Ctrl Pts',(-1.63979664655005,-1.82099346730383,
94.1989634876225));
#11675=CARTESIAN_POINT('Ctrl Pts',(-1.57955671189084,-1.87523926478536,
94.2031876334481));
#11676=CARTESIAN_POINT('Ctrl Pts',(-1.51653167006043,-1.926574137586,94.2074117792738));
#11677=CARTESIAN_POINT('Ctrl Pts',(-1.45103566161278,-1.97470143533851,
94.2116359250994));
#11678=CARTESIAN_POINT('Ctrl Pts',(-1.38520112752636,-2.02307748602421,
94.2158819040366));
#11679=CARTESIAN_POINT('Ctrl Pts',(-1.31687032778023,-2.06821235319246,
94.2201278829739));
#11680=CARTESIAN_POINT('Ctrl Pts',(-1.24639803252967,-2.10984411616265,
94.2243738619112));
#11681=CARTESIAN_POINT('Ctrl Pts',(-1.17641500285063,-2.15118684372921,
94.2285903624371));
#11682=CARTESIAN_POINT('Ctrl Pts',(-1.10432052466984,-2.18907471509843,
94.2328068629629));
#11683=CARTESIAN_POINT('Ctrl Pts',(-1.03049163928184,-2.22329422959945,
94.2370233634888));
#11684=CARTESIAN_POINT('Ctrl Pts',(-0.956687319393937,-2.25750235804904,
94.2412384610348));
#11685=CARTESIAN_POINT('Ctrl Pts',(-0.881150160021461,-2.28804435802382,
94.2454535585807));
#11686=CARTESIAN_POINT('Ctrl Pts',(-0.804280365001129,-2.31475340899925,
94.2496686561267));
#11687=CARTESIAN_POINT('Ctrl Pts',(-0.727412566168601,-2.34146176638259,
94.2538836442132));
#11688=CARTESIAN_POINT('Ctrl Pts',(-0.649212640259519,-2.36433722099284,
94.2580986322996));
#11689=CARTESIAN_POINT('Ctrl Pts',(-0.570097896893327,-2.38326218405735,
94.2623136203861));
#11690=CARTESIAN_POINT('Ctrl Pts',(-0.489972799761986,-2.40242883289209,
94.2665824369868));
#11691=CARTESIAN_POINT('Ctrl Pts',(-0.408909824615682,-2.41754324086638,
94.2708512535874));
#11692=CARTESIAN_POINT('Ctrl Pts',(-0.327353328602962,-2.42853660632336,
94.2751200701881));
#11693=CARTESIAN_POINT('Ctrl Pts',(-0.246707785834168,-2.43940718031167,
94.279341205825));
#11694=CARTESIAN_POINT('Ctrl Pts',(-0.165580166612593,-2.44624833644876,
94.2835623414619));
#11695=CARTESIAN_POINT('Ctrl Pts',(-0.0844035797152592,-2.44904599502158,
94.2877834770988));
#11696=CARTESIAN_POINT('Ctrl Pts',(-0.00185156512608912,-2.4518910561426,
94.2920761341813));
#11697=CARTESIAN_POINT('Ctrl Pts',(0.0807505892343749,-2.45055433345196,
94.2963687912638));
#11698=CARTESIAN_POINT('Ctrl Pts',(0.162951184608371,-2.4450761054484,94.3006614483463));
#11699=CARTESIAN_POINT('Ctrl Pts',(0.245151779982366,-2.43959787744484,
94.3049541054288));
#11700=CARTESIAN_POINT('Ctrl Pts',(0.326950328938398,-2.42997826853912,
94.3092467625113));
#11701=CARTESIAN_POINT('Ctrl Pts',(0.407906368883997,-2.41631178539192,
94.3135394195939));
#11702=CARTESIAN_POINT('Ctrl Pts',(0.487685163948704,-2.40284403722898,
94.3177696538037));
#11703=CARTESIAN_POINT('Ctrl Pts',(0.566946691320933,-2.38539558823848,
94.3219998880135));
#11704=CARTESIAN_POINT('Ctrl Pts',(0.64526306635131,-2.36401899848603,94.3262301222233));
#11705=CARTESIAN_POINT('Ctrl Pts',(0.72346672490408,-2.34267317489072,94.3304542680882));
#11706=CARTESIAN_POINT('Ctrl Pts',(0.800727487791892,-2.31741056015666,
94.3346784139532));
#11707=CARTESIAN_POINT('Ctrl Pts',(0.876625954662874,-2.28833502477487,
94.3389025598181));
#11708=CARTESIAN_POINT('Ctrl Pts',(0.952916712904789,-2.2591092086021,94.3431485387456));
#11709=CARTESIAN_POINT('Ctrl Pts',(1.02783058150085,-2.226031018153,94.3473945176731));
#11710=CARTESIAN_POINT('Ctrl Pts',(1.10095540803066,-2.18925728034145,94.3516404966005));
#11711=CARTESIAN_POINT('Ctrl Pts',(1.17357255420321,-2.1527388498617,94.3558569971661));
#11712=CARTESIAN_POINT('Ctrl Pts',(1.24442499997529,-2.11257623508412,94.3600734977317));
#11713=CARTESIAN_POINT('Ctrl Pts',(1.31312928358055,-2.06897117780873,94.3642899982973));
#11714=CARTESIAN_POINT('Ctrl Pts',(1.38181070682456,-2.02538062948837,94.368505095883));
#11715=CARTESIAN_POINT('Ctrl Pts',(1.44834499484991,-1.97835016233186,94.3727201934688));
#11716=CARTESIAN_POINT('Ctrl Pts',(1.51237543097266,-1.92812624218184,94.3769352910545));
#11717=CARTESIAN_POINT('Ctrl Pts',(1.57640420432572,-1.87790362626801,94.3811502791808));
#11718=CARTESIAN_POINT('Ctrl Pts',(1.6379288896881,-1.82448801017855,94.385365267307));
#11719=CARTESIAN_POINT('Ctrl Pts',(1.69662493671454,-1.76816686828998,94.3895802554333));
#11720=CARTESIAN_POINT('Ctrl Pts',(1.7560705744423,-1.71112646494537,94.3938490719869));
#11721=CARTESIAN_POINT('Ctrl Pts',(1.81261444802059,-1.65110612281475,94.3981178885406));
#11722=CARTESIAN_POINT('Ctrl Pts',(1.86595842410606,-1.58844244765356,94.4023867050943));
#11723=CARTESIAN_POINT('Ctrl Pts',(1.91870657051599,-1.52647869926911,94.4066078407706));
#11724=CARTESIAN_POINT('Ctrl Pts',(1.96832570872978,-1.46193078482751,94.4108289764469));
#11725=CARTESIAN_POINT('Ctrl Pts',(2.01456982077987,-1.39515543478243,94.4150501121232));
#11726=CARTESIAN_POINT('Ctrl Pts',(2.06159747546096,-1.32724866862533,94.4193427691155));
#11727=CARTESIAN_POINT('Ctrl Pts',(2.10513440770179,-1.2570387122475,94.4236354261079));
#11728=CARTESIAN_POINT('Ctrl Pts',(2.14497027593332,-1.18492732492863,94.4279280831002));
#11729=CARTESIAN_POINT('Ctrl Pts',(2.18480614416486,-1.11281593760977,94.4322207400926));
#11730=CARTESIAN_POINT('Ctrl Pts',(2.22094078949991,-1.03880359665717,94.4365133970849));
#11731=CARTESIAN_POINT('Ctrl Pts',(2.25321556377465,-0.963311929316616,
94.4408060540773));
#11732=CARTESIAN_POINT('Ctrl Pts',(2.28502100500606,-0.888918046074483,
94.445036288146));
#11733=CARTESIAN_POINT('Ctrl Pts',(2.3131980940021,-0.81280701318249,94.4492665222147));
#11734=CARTESIAN_POINT('Ctrl Pts',(2.33755969660922,-0.735367197247882,
94.4534967562834));
#11735=CARTESIAN_POINT('Ctrl Pts',(2.36188623689144,-0.658038836213461,
94.4577209020072));
#11736=CARTESIAN_POINT('Ctrl Pts',(2.38240805854403,-0.579385930284001,
94.4619450477309));
#11737=CARTESIAN_POINT('Ctrl Pts',(2.39898577846083,-0.499817451418697,
94.4661691934546));
#11738=CARTESIAN_POINT('Ctrl Pts',(2.41564918323451,-0.419837708896056,
94.4704151724173));
#11739=CARTESIAN_POINT('Ctrl Pts',(2.4283274059592,-0.338933338094459,94.4746611513801));
#11740=CARTESIAN_POINT('Ctrl Pts',(2.43692953074504,-0.257535846403518,
94.4789071303429));
#11741=CARTESIAN_POINT('Ctrl Pts',(2.4454719336006,-0.176703472685579,94.483123630768));
#11742=CARTESIAN_POINT('Ctrl Pts',(2.44999460796228,-0.0953852722739111,
94.4873401311931));
#11743=CARTESIAN_POINT('Ctrl Pts',(2.45045993409078,-0.0140129017627399,
94.4915566316182));
#11744=CARTESIAN_POINT('Ctrl Pts',(2.45092510538877,0.0673323932739367,
94.495771729064));
#11745=CARTESIAN_POINT('Ctrl Pts',(2.44733560667782,0.148731357811173,94.4999868265098));
#11746=CARTESIAN_POINT('Ctrl Pts',(2.43970590188025,0.229750652514127,94.5042019239556));
#11747=CARTESIAN_POINT('Ctrl Pts',(2.43207639521272,0.310767843288186,94.5084169119428));
#11748=CARTESIAN_POINT('Ctrl Pts',(2.42040693573168,0.391404920793907,94.5126318999299));
#11749=CARTESIAN_POINT('Ctrl Pts',(2.40476387660299,0.471233432372271,94.516846887917));
#11750=CARTESIAN_POINT('Ctrl Pts',(2.38892104322614,0.552081417235941,94.5211157046374));
#11751=CARTESIAN_POINT('Ctrl Pts',(2.36900247361349,0.632099554290949,94.5253845213577));
#11752=CARTESIAN_POINT('Ctrl Pts',(2.34513013480676,0.710855049093141,94.529653338078));
#11753=CARTESIAN_POINT('Ctrl Pts',(2.32152444161996,0.788730872745221,94.5338744736185));
#11754=CARTESIAN_POINT('Ctrl Pts',(2.29405308119321,0.865371697897479,94.5380956091589));
#11755=CARTESIAN_POINT('Ctrl Pts',(2.26288312779351,0.940377690051954,94.5423167446994));
#11756=CARTESIAN_POINT('Ctrl Pts',(2.23118503920108,1.01665456328908,94.5466094020097));
#11757=CARTESIAN_POINT('Ctrl Pts',(2.19566207516387,1.0912402353514,94.5509020593199));
#11758=CARTESIAN_POINT('Ctrl Pts',(2.15653847906908,1.16374053735978,94.5551947166302));
#11759=CARTESIAN_POINT('Ctrl Pts',(2.11741488297429,1.23624083936815,94.5594873739404));
#11760=CARTESIAN_POINT('Ctrl Pts',(2.07469097043895,1.30665537959105,94.5637800312507));
#11761=CARTESIAN_POINT('Ctrl Pts',(2.02863564799526,1.37462273285541,94.568072688561));
#11762=CARTESIAN_POINT('Ctrl Pts',(1.98325005421671,1.44160171642957,94.5723029227788));
#11763=CARTESIAN_POINT('Ctrl Pts',(1.93445816508792,1.50645685988666,94.5765331569966));
#11764=CARTESIAN_POINT('Ctrl Pts',(1.88248550546635,1.56882075831151,94.5807633912144));
#11765=CARTESIAN_POINT('Ctrl Pts',(1.83058764726583,1.63109489977072,94.5849875370863));
#11766=CARTESIAN_POINT('Ctrl Pts',(1.7755184057447,1.69088456284987,94.5892116829582));
#11767=CARTESIAN_POINT('Ctrl Pts',(1.71754645763939,1.74785137121278,94.5934358288301));
#11768=CARTESIAN_POINT('Ctrl Pts',(1.65927487389282,1.80511262001994,94.5976818077557));
#11769=CARTESIAN_POINT('Ctrl Pts',(1.59807075486495,1.85952135251601,94.6019277866813));
#11770=CARTESIAN_POINT('Ctrl Pts',(1.53424793998413,1.91076777988704,94.6061737656069));
#11771=CARTESIAN_POINT('Ctrl Pts',(1.47086822472033,1.96165842112761,94.6103902661769));
#11772=CARTESIAN_POINT('Ctrl Pts',(1.40490642735054,2.00943023267578,94.6146067667468));
#11773=CARTESIAN_POINT('Ctrl Pts',(1.3367053290778,2.05381817920064,94.6188232673168));
#11774=CARTESIAN_POINT('Ctrl Pts',(1.26852692375421,2.09819135626519,94.6230383649059));
#11775=CARTESIAN_POINT('Ctrl Pts',(1.19811108671214,2.13918265064091,94.627253462495));
#11776=CARTESIAN_POINT('Ctrl Pts',(1.12583017537303,2.17656993138735,94.6314685600842));
#11777=CARTESIAN_POINT('Ctrl Pts',(1.05355114107204,2.21395624123636,94.6356835482129));
#11778=CARTESIAN_POINT('Ctrl Pts',(0.979407542444483,2.24773851076299,94.6398985363416));
#11779=CARTESIAN_POINT('Ctrl Pts',(0.903795681637717,2.27774090182642,94.6441135244703));
#11780=CARTESIAN_POINT('Ctrl Pts',(0.827218203179831,2.30812644492548,94.6483823410182));
#11781=CARTESIAN_POINT('Ctrl Pts',(0.749135142350709,2.33463468329617,94.652651157566));
#11782=CARTESIAN_POINT('Ctrl Pts',(0.669976523004302,2.35713421523321,94.6569199741139));
#11783=CARTESIAN_POINT('Ctrl Pts',(0.591702071884836,2.37938243693487,94.6611411097902));
#11784=CARTESIAN_POINT('Ctrl Pts',(0.512376442463163,2.39771101188027,94.6653622454666));
#11785=CARTESIAN_POINT('Ctrl Pts',(0.432426320493267,2.41204430459821,94.6695833811429));
#11786=CARTESIAN_POINT('Ctrl Pts',(0.351121554257427,2.42662045514192,94.6738760381266));
#11787=CARTESIAN_POINT('Ctrl Pts',(0.269171435538037,2.43706461483055,94.6781686951102));
#11788=CARTESIAN_POINT('Ctrl Pts',(0.187028794132821,2.44335230373461,94.6824613520938));
#11789=CARTESIAN_POINT('Ctrl Pts',(0.104886152727603,2.44963999263867,94.6867540090774));
#11790=CARTESIAN_POINT('Ctrl Pts',(0.0225514888198296,2.45177126446202,
94.691046666061));
#11791=CARTESIAN_POINT('Ctrl Pts',(-0.0595257641802243,2.44977691502691,
94.6953393230447));
#11792=CARTESIAN_POINT('Ctrl Pts',(-0.140409474789221,2.44781156681328,
94.6995695575191));
#11793=CARTESIAN_POINT('Ctrl Pts',(-0.221348271614469,2.4418324280466,94.7037997919935));
#11794=CARTESIAN_POINT('Ctrl Pts',(-0.301911146407717,2.43183056763311,
94.7080300264679));
#11795=CARTESIAN_POINT('Ctrl Pts',(-0.382358071494822,2.42184310234614,
94.712254172599));
#11796=CARTESIAN_POINT('Ctrl Pts',(-0.462429691378725,2.4078444707579,94.71647831873));
#11797=CARTESIAN_POINT('Ctrl Pts',(-0.541696086056398,2.38987773753202,
94.7207024648611));
#11798=CARTESIAN_POINT('Ctrl Pts',(-0.62137217342591,2.3718181422638,94.7249484437222));
#11799=CARTESIAN_POINT('Ctrl Pts',(-0.700234211369373,2.34974931577968,
94.7291944225834));
#11800=CARTESIAN_POINT('Ctrl Pts',(-0.77785190998881,2.32376777155695,94.7334404014445));
#11801=CARTESIAN_POINT('Ctrl Pts',(-0.854930741895584,2.29796660615985,
94.7376569022779));
#11802=CARTESIAN_POINT('Ctrl Pts',(-0.930782010665086,2.26830702926195,
94.7418734031114));
#11803=CARTESIAN_POINT('Ctrl Pts',(-1.00499742590154,2.23493409834189,94.7460899039448));
#11804=CARTESIAN_POINT('Ctrl Pts',(-1.07918814702948,2.20157227178303,94.7503050017984));
#11805=CARTESIAN_POINT('Ctrl Pts',(-1.15174367158573,2.16449973542075,94.754520099652));
#11806=CARTESIAN_POINT('Ctrl Pts',(-1.22227581023555,2.12390962465756,94.7587351975056));
#11807=CARTESIAN_POINT('Ctrl Pts',(-1.29280611727141,2.08332056795873,94.7629501858995));
#11808=CARTESIAN_POINT('Ctrl Pts',(-1.36131274021397,2.03921435142673,94.7671651742933));
#11809=CARTESIAN_POINT('Ctrl Pts',(-1.42743348605354,1.99182928306947,94.7713801626871));
#11810=CARTESIAN_POINT('Ctrl Pts',(-1.49439863211182,1.94383907994586,94.7756489789239));
#11811=CARTESIAN_POINT('Ctrl Pts',(-1.55891612237586,1.89248595458735,94.7799177951607));
#11812=CARTESIAN_POINT('Ctrl Pts',(-1.6206429124431,1.83806060845337,94.7841866113974));
#11813=CARTESIAN_POINT('Ctrl Pts',(-1.6816802486939,1.78424316307952,94.7884077473378));
#11814=CARTESIAN_POINT('Ctrl Pts',(-1.73998862154228,1.72742215829781,94.7926288832782));
#11815=CARTESIAN_POINT('Ctrl Pts',(-1.79527370339053,1.66791563932786,94.7968500192185));
#11816=CARTESIAN_POINT('Ctrl Pts',(-1.85149550314817,1.60740087690087,94.8011426756035));
#11817=CARTESIAN_POINT('Ctrl Pts',(-1.90459028865089,1.54410913767614,94.8054353319885));
#11818=CARTESIAN_POINT('Ctrl Pts',(-1.95429263032105,1.47840811857648,94.8097279883734));
#11819=CARTESIAN_POINT('Ctrl Pts',(-2.00399497199121,1.41270709947681,94.8140206447584));
#11820=CARTESIAN_POINT('Ctrl Pts',(-2.05030464456659,1.34459725030632,94.8183133011434));
#11821=CARTESIAN_POINT('Ctrl Pts',(-2.09300455428211,1.27447329738773,94.8226059575283));
#11822=CARTESIAN_POINT('Ctrl Pts',(-2.13642069144977,1.2031731194966,94.8269706168371));
#11823=CARTESIAN_POINT('Ctrl Pts',(-2.17626044123707,1.12953615291983,94.8313352761459));
#11824=CARTESIAN_POINT('Ctrl Pts',(-2.2122733453413,1.05394349729595,94.8356999354546));
#11825=CARTESIAN_POINT('Ctrl Pts',(-2.24822307132856,0.978483455293714,
94.8400569377592));
#11826=CARTESIAN_POINT('Ctrl Pts',(-2.28035912062873,0.901074927510781,
94.8444139400638));
#11827=CARTESIAN_POINT('Ctrl Pts',(-2.30847555175356,0.822125827933955,
94.8487709423684));
#11828=CARTESIAN_POINT('Ctrl Pts',(-2.33653701668684,0.743331069827807,
94.8531194269553));
#11829=CARTESIAN_POINT('Ctrl Pts',(-2.36059436775562,0.663002134486998,
94.8574679115423));
#11830=CARTESIAN_POINT('Ctrl Pts',(-2.3804892538109,0.581567848570437,94.8618163961292));
#11831=CARTESIAN_POINT('Ctrl Pts',(-2.40036100275622,0.500228268098339,
94.8661598235689));
#11832=CARTESIAN_POINT('Ctrl Pts',(-2.41607981075422,0.417786303621603,
94.8705032510087));
#11833=CARTESIAN_POINT('Ctrl Pts',(-2.42753682224339,0.334686759003764,
94.8748466784485));
#11834=CARTESIAN_POINT('Ctrl Pts',(-2.43898051632255,0.25168380769989,94.8791850571716));
#11835=CARTESIAN_POINT('Ctrl Pts',(-2.4461722172272,0.168025217525998,94.8835234358948));
#11836=CARTESIAN_POINT('Ctrl Pts',(-2.44905418491344,0.0841656067402018,
94.887861814618));
#11837=CARTESIAN_POINT('Ctrl Pts',(-2.45002501882,0.0559162429704074,94.8893232623587));
#11838=CARTESIAN_POINT('Ctrl Pts',(-2.45050722465988,0.0276441353787134,
94.8907847100995));
#11839=CARTESIAN_POINT('Ctrl Pts',(-2.45049991819823,-0.00063317491965548,
94.8922461578402));
#11840=CARTESIAN_POINT('',(-2.45049916761641,-0.00201978001007516,95.6922461577976));
#11841=CARTESIAN_POINT('Ctrl Pts',(-2.45049991819808,-0.000633175507850709,
94.8922461578706));
#11842=CARTESIAN_POINT('Ctrl Pts',(-2.45047735789977,-0.0879454743182435,
94.8967586932033));
#11843=CARTESIAN_POINT('Ctrl Pts',(-2.44578411198309,-0.175130467335658,
94.901271228536));
#11844=CARTESIAN_POINT('Ctrl Pts',(-2.43648610108198,-0.261697782249549,
94.9057837638687));
#11845=CARTESIAN_POINT('Ctrl Pts',(-2.42715182304631,-0.348602755238054,
94.9103139004635));
#11846=CARTESIAN_POINT('Ctrl Pts',(-2.41317689096561,-0.434884875770232,
94.9148440370582));
#11847=CARTESIAN_POINT('Ctrl Pts',(-2.3946786543609,-0.520061912033822,
94.919374173653));
#11848=CARTESIAN_POINT('Ctrl Pts',(-2.37614175994702,-0.605416952162517,
94.9239137773747));
#11849=CARTESIAN_POINT('Ctrl Pts',(-2.35306278731216,-0.689661956551622,
94.9284533810965));
#11850=CARTESIAN_POINT('Ctrl Pts',(-2.32560864957564,-0.772330666890149,
94.9329929848183));
#11851=CARTESIAN_POINT('Ctrl Pts',(-2.2980712145746,-0.855250198343442,
94.937546361931));
#11852=CARTESIAN_POINT('Ctrl Pts',(-2.26613220165545,-0.9365835419457,94.9420997390438));
#11853=CARTESIAN_POINT('Ctrl Pts',(-2.23000666024073,-1.0158841200068,94.9466531161565));
#11854=CARTESIAN_POINT('Ctrl Pts',(-2.22149244427397,-1.03457400592851,
94.947726274775));
#11855=CARTESIAN_POINT('Ctrl Pts',(-2.2127458756019,-1.05315109379866,94.9487994333934));
#11856=CARTESIAN_POINT('Ctrl Pts',(-2.20377012755118,-1.07160975868693,
94.9498725920119));
#11857=CARTESIAN_POINT('Ctrl Pts',(-2.16838903720358,-1.14437112480566,
94.9541028268427));
#11858=CARTESIAN_POINT('Ctrl Pts',(-2.12933383572574,-1.21551556172193,
94.9583330616736));
#11859=CARTESIAN_POINT('Ctrl Pts',(-2.08677540852799,-1.2846472840289,94.9625632965045));
#11860=CARTESIAN_POINT('Ctrl Pts',(-2.04427823340945,-1.35367950872731,
94.9667874429835));
#11861=CARTESIAN_POINT('Ctrl Pts',(-1.99828808797043,-1.42070437919437,
94.9710115894625));
#11862=CARTESIAN_POINT('Ctrl Pts',(-1.94902270471539,-1.48534869525776,
94.9752357359415));
#11863=CARTESIAN_POINT('Ctrl Pts',(-1.89950269574123,-1.55032712230084,
94.9794817147146));
#11864=CARTESIAN_POINT('Ctrl Pts',(-1.84667370015972,-1.61289988602724,
94.9837276934877));
#11865=CARTESIAN_POINT('Ctrl Pts',(-1.790802224898,-1.67271564866846,94.9879736722608));
#11866=CARTESIAN_POINT('Ctrl Pts',(-1.73531863612909,-1.73211614168818,
94.9921901734192));
#11867=CARTESIAN_POINT('Ctrl Pts',(-1.67683500032028,-1.7887974488079,94.9964066745777));
#11868=CARTESIAN_POINT('Ctrl Pts',(-1.61565284657833,-1.84244840615507,
95.0006231757362));
#11869=CARTESIAN_POINT('Ctrl Pts',(-1.55449105044771,-1.89608151180413,
95.0048382739057));
#11870=CARTESIAN_POINT('Ctrl Pts',(-1.49063286891244,-1.94668596353109,
95.0090533720751));
#11871=CARTESIAN_POINT('Ctrl Pts',(-1.4244152176806,-1.9939888509317,95.0132684702445));
#11872=CARTESIAN_POINT('Ctrl Pts',(-1.35819928617254,-2.04129050983962,
95.0174834589446));
#11873=CARTESIAN_POINT('Ctrl Pts',(-1.28962438594445,-2.08529050536559,
95.0216984476447));
#11874=CARTESIAN_POINT('Ctrl Pts',(-1.21905772795312,-2.12575833666901,
95.0259134363447));
#11875=CARTESIAN_POINT('Ctrl Pts',(-1.14758990460616,-2.1667429588851,95.0301822521906));
#11876=CARTESIAN_POINT('Ctrl Pts',(-1.07407950609926,-2.20410430293818,
95.0344510680365));
#11877=CARTESIAN_POINT('Ctrl Pts',(-0.998933451089233,-2.23765104748148,
95.0387198838824));
#11878=CARTESIAN_POINT('Ctrl Pts',(-0.924626723872426,-2.27082309883478,
95.0429410201025));
#11879=CARTESIAN_POINT('Ctrl Pts',(-0.848721157933712,-2.30026522668508,
95.0471621563226));
#11880=CARTESIAN_POINT('Ctrl Pts',(-0.771628312528639,-2.32584178251751,
95.0513832925427));
#11881=CARTESIAN_POINT('Ctrl Pts',(-0.693229269752938,-2.35185168634484,
95.0556759482015));
#11882=CARTESIAN_POINT('Ctrl Pts',(-0.613602826292481,-2.37386367892888,
95.0599686038603));
#11883=CARTESIAN_POINT('Ctrl Pts',(-0.533193705700807,-2.39178902125606,
95.0642612595191));
#11884=CARTESIAN_POINT('Ctrl Pts',(-0.452784585109126,-2.40971436358325,
95.0685539151779));
#11885=CARTESIAN_POINT('Ctrl Pts',(-0.371593290117368,-2.42355303755492,
95.0728465708367));
#11886=CARTESIAN_POINT('Ctrl Pts',(-0.290069056961055,-2.43327149989345,
95.0771392264955));
#11887=CARTESIAN_POINT('Ctrl Pts',(-0.209730264145545,-2.44284864649234,
95.0813694628345));
#11888=CARTESIAN_POINT('Ctrl Pts',(-0.128765155128878,-2.4484607827584,
95.0855996991734));
#11889=CARTESIAN_POINT('Ctrl Pts',(-0.0475990703908773,-2.45003766879163,
95.0898299355123));
#11890=CARTESIAN_POINT('Ctrl Pts',(0.0334501967872597,-2.45161228530577,
95.0940540835215));
#11891=CARTESIAN_POINT('Ctrl Pts',(0.114699404089822,-2.44916317693098,
95.0982782315307));
#11892=CARTESIAN_POINT('Ctrl Pts',(0.19571688106442,-2.44267172425326,95.1025023795399));
#11893=CARTESIAN_POINT('Ctrl Pts',(0.277153056114405,-2.43614672376779,
95.1067483579332));
#11894=CARTESIAN_POINT('Ctrl Pts',(0.35835462605696,-2.42553741631223,95.1109943363265));
#11895=CARTESIAN_POINT('Ctrl Pts',(0.438881940923745,-2.41087803340007,
95.1152403147198));
#11896=CARTESIAN_POINT('Ctrl Pts',(0.518850233643703,-2.39632041620208,
95.1194568174506));
#11897=CARTESIAN_POINT('Ctrl Pts',(0.598153139337098,-2.37776886130359,
95.1236733201814));
#11898=CARTESIAN_POINT('Ctrl Pts',(0.676365867025972,-2.35530878313698,
95.1278898229122));
#11899=CARTESIAN_POINT('Ctrl Pts',(0.754552570625387,-2.33285617821802,
95.1321049226661));
#11900=CARTESIAN_POINT('Ctrl Pts',(0.831649369793658,-2.30649776086538,
95.1363200224201));
#11901=CARTESIAN_POINT('Ctrl Pts',(0.907244520584572,-2.27636939662026,
95.140535122174));
#11902=CARTESIAN_POINT('Ctrl Pts',(0.982837708291136,-2.24624181476024,
95.1447501124686));
#11903=CARTESIAN_POINT('Ctrl Pts',(1.05692889341685,-2.21234465386775,95.1489651027632));
#11904=CARTESIAN_POINT('Ctrl Pts',(1.12912562806165,-2.17486219472738,95.1531800930578));
#11905=CARTESIAN_POINT('Ctrl Pts',(1.20224428542304,-2.13690109994337,95.1574489070513));
#11906=CARTESIAN_POINT('Ctrl Pts',(1.27341932385271,-2.09526270025244,95.1617177210447));
#11907=CARTESIAN_POINT('Ctrl Pts',(1.34226978604317,-2.05018586266602,95.1659865350381));
#11908=CARTESIAN_POINT('Ctrl Pts',(1.41035129310837,-2.00561246491414,95.1702076728607));
#11909=CARTESIAN_POINT('Ctrl Pts',(1.47615954531245,-1.95767737856541,95.1744288106833));
#11910=CARTESIAN_POINT('Ctrl Pts',(1.53935790885744,-1.90665347623475,95.1786499485059));
#11911=CARTESIAN_POINT('Ctrl Pts',(1.60362697517438,-1.85476513010211,95.1829426005848));
#11912=CARTESIAN_POINT('Ctrl Pts',(1.66519652468833,-1.7996826712849,95.1872352526637));
#11913=CARTESIAN_POINT('Ctrl Pts',(1.72375145497051,-1.74173223300456,95.1915279047425));
#11914=CARTESIAN_POINT('Ctrl Pts',(1.7823063852527,-1.68378179472421,95.1958205568214));
#11915=CARTESIAN_POINT('Ctrl Pts',(1.83784640926265,-1.62296379010353,95.2001132089003));
#11916=CARTESIAN_POINT('Ctrl Pts',(1.89010041660449,-1.55963799169921,95.2044058609792));
#11917=CARTESIAN_POINT('Ctrl Pts',(1.94159452572965,-1.4972331018285,95.2086360876322));
#11918=CARTESIAN_POINT('Ctrl Pts',(1.99009181235062,-1.43215754003063,95.2128663142852));
#11919=CARTESIAN_POINT('Ctrl Pts',(2.03530321545965,-1.36473113511035,95.2170965409383));
#11920=CARTESIAN_POINT('Ctrl Pts',(2.08044954808959,-1.2974017735944,95.2213206792407));
#11921=CARTESIAN_POINT('Ctrl Pts',(2.12231913272111,-1.22772867168445,95.2255448175431));
#11922=CARTESIAN_POINT('Ctrl Pts',(2.16066291033438,-1.15606489346635,95.2297689558455));
#11923=CARTESIAN_POINT('Ctrl Pts',(2.19920495904508,-1.08403055040467,95.2340149366629));
#11924=CARTESIAN_POINT('Ctrl Pts',(2.23418432595282,-1.00998524945895,95.2382609174803));
#11925=CARTESIAN_POINT('Ctrl Pts',(2.26539209553103,-0.934317346251,95.2425068982977));
#11926=CARTESIAN_POINT('Ctrl Pts',(2.29638313128798,-0.859174946596514,
95.2467233913414));
#11927=CARTESIAN_POINT('Ctrl Pts',(2.32365461055945,-0.782432846519269,
95.250939884385));
#11928=CARTESIAN_POINT('Ctrl Pts',(2.34704871011201,-0.704494572272601,
95.2551563774287));
#11929=CARTESIAN_POINT('Ctrl Pts',(2.37043502577665,-0.626582230325246,
95.2593714675242));
#11930=CARTESIAN_POINT('Ctrl Pts',(2.38994639000836,-0.547474949753931,
95.2635865576197));
#11931=CARTESIAN_POINT('Ctrl Pts',(2.40547447471462,-0.467592559282576,
95.2678016477152));
#11932=CARTESIAN_POINT('Ctrl Pts',(2.42100215633336,-0.387712242447165,
95.2720166283928));
#11933=CARTESIAN_POINT('Ctrl Pts',(2.43254667629042,-0.307057312559571,
95.2762316090704));
#11934=CARTESIAN_POINT('Ctrl Pts',(2.44005086774202,-0.226057543186284,
95.280446589748));
#11935=CARTESIAN_POINT('Ctrl Pts',(2.44765092242728,-0.144023032113256,
95.2847154152243));
#11936=CARTESIAN_POINT('Ctrl Pts',(2.45110662479623,-0.0616352936289753,
95.2889842407005));
#11937=CARTESIAN_POINT('Ctrl Pts',(2.45041294026594,0.0206560445693769,
95.2932530661767));
#11938=CARTESIAN_POINT('Ctrl Pts',(2.44972700651406,0.102027913037481,95.2974741945819));
#11939=CARTESIAN_POINT('Ctrl Pts',(2.44498403849069,0.18330505823126,95.301695322987));
#11940=CARTESIAN_POINT('Ctrl Pts',(2.43623157313892,0.264056759127766,95.3059164513921));
#11941=CARTESIAN_POINT('Ctrl Pts',(2.42733075872425,0.34617715314952,95.3102091254039));
#11942=CARTESIAN_POINT('Ctrl Pts',(2.41428334790203,0.427753629191953,95.3145017994157));
#11943=CARTESIAN_POINT('Ctrl Pts',(2.39719332599091,0.50834477259496,95.3187944734275));
#11944=CARTESIAN_POINT('Ctrl Pts',(2.3801033040798,0.588935915997967,95.3230871474393));
#11945=CARTESIAN_POINT('Ctrl Pts',(2.35897086342322,0.668541261909216,95.3273798214511));
#11946=CARTESIAN_POINT('Ctrl Pts',(2.3339520747727,0.746738215617897,95.3316724954629));
#11947=CARTESIAN_POINT('Ctrl Pts',(2.30929715729089,0.823797879374917,95.335902737183));
#11948=CARTESIAN_POINT('Ctrl Pts',(2.28077524768402,0.899780502572685,95.3401329789031));
#11949=CARTESIAN_POINT('Ctrl Pts',(2.24849910680534,0.974269991683817,95.3443632206233));
#11950=CARTESIAN_POINT('Ctrl Pts',(2.21626941952085,1.04865227143212,95.3485873739473));
#11951=CARTESIAN_POINT('Ctrl Pts',(2.18029641548116,1.12154526189137,95.3528115272713));
#11952=CARTESIAN_POINT('Ctrl Pts',(2.14074244224802,1.19254855077602,95.3570356805952));
#11953=CARTESIAN_POINT('Ctrl Pts',(2.1009841167441,1.26391867217156,95.3612816576515));
#11954=CARTESIAN_POINT('Ctrl Pts',(2.0576078550931,1.33337905458774,95.3655276347078));
#11955=CARTESIAN_POINT('Ctrl Pts',(2.01082739494091,1.40054397922919,95.3697736117641));
#11956=CARTESIAN_POINT('Ctrl Pts',(1.96437161462644,1.46724274563359,95.3739901196118));
#11957=CARTESIAN_POINT('Ctrl Pts',(1.91455900926562,1.53167742989576,95.3782066274594));
#11958=CARTESIAN_POINT('Ctrl Pts',(1.86164370577044,1.59349708589796,95.3824231353071));
#11959=CARTESIAN_POINT('Ctrl Pts',(1.80874601007896,1.65529617113339,95.3866382400929));
#11960=CARTESIAN_POINT('Ctrl Pts',(1.75274796872534,1.71448160296329,95.3908533448786));
#11961=CARTESIAN_POINT('Ctrl Pts',(1.69394418380189,1.77073525750287,95.3950684496645));
#11962=CARTESIAN_POINT('Ctrl Pts',(1.63514192718873,1.82698745001004,95.3992834448997));
#11963=CARTESIAN_POINT('Ctrl Pts',(1.57353440886822,1.88030769592763,95.4034984401349));
#11964=CARTESIAN_POINT('Ctrl Pts',(1.5094522587701,1.93041553259754,95.4077134353702));
#11965=CARTESIAN_POINT('Ctrl Pts',(1.44455197487279,1.98116309366373,95.4119822432515));
#11966=CARTESIAN_POINT('Ctrl Pts',(1.37711379745793,2.02861532240687,95.4162510511329));
#11967=CARTESIAN_POINT('Ctrl Pts',(1.30751323677533,2.0725248817945,95.4205198590142));
#11968=CARTESIAN_POINT('Ctrl Pts',(1.23868983402477,2.11594414825868,95.4247410015051));
#11969=CARTESIAN_POINT('Ctrl Pts',(1.16775253861468,2.1558992892507,95.4289621439959));
#11970=CARTESIAN_POINT('Ctrl Pts',(1.09508938887755,2.19219740907788,95.4331832864868));
#11971=CARTESIAN_POINT('Ctrl Pts',(1.02119546426745,2.2291103496771,95.4374759270634));
#11972=CARTESIAN_POINT('Ctrl Pts',(0.945517138300447,2.26224103266617,95.44176856764));
#11973=CARTESIAN_POINT('Ctrl Pts',(0.868481951697543,2.29143827095028,95.4460612082166));
#11974=CARTESIAN_POINT('Ctrl Pts',(0.79144676509464,2.3206355092344,95.4503538487932));
#11975=CARTESIAN_POINT('Ctrl Pts',(0.713055212866924,2.34589921328184,95.4546464893698));
#11976=CARTESIAN_POINT('Ctrl Pts',(0.633747165398412,2.36713218480707,95.4589391299464));
#11977=CARTESIAN_POINT('Ctrl Pts',(0.555591830508406,2.38805654309395,95.4631693786102));
#11978=CARTESIAN_POINT('Ctrl Pts',(0.476251723940673,2.40514552681904,95.4673996272739));
#11979=CARTESIAN_POINT('Ctrl Pts',(0.39613784477759,2.41826902100138,95.4716298759377));
#11980=CARTESIAN_POINT('Ctrl Pts',(0.316139266183492,2.43137362774046,95.4758540363919));
#11981=CARTESIAN_POINT('Ctrl Pts',(0.235369581833704,2.44052400502367,95.4800781968462));
#11982=CARTESIAN_POINT('Ctrl Pts',(0.154253409653161,2.4456402302077,95.4843023573005));
#11983=CARTESIAN_POINT('Ctrl Pts',(0.0727183290141794,2.45078287712672,
95.4885483325975));
#11984=CARTESIAN_POINT('Ctrl Pts',(-0.00916636924427454,2.45184945747314,
95.4927943078946));
#11985=CARTESIAN_POINT('Ctrl Pts',(-0.0909606451694004,2.44881122404941,
95.4970402831917));
#11986=CARTESIAN_POINT('Ctrl Pts',(-0.172187406493778,2.44579407085176,
95.5012567985669));
#11987=CARTESIAN_POINT('Ctrl Pts',(-0.253324525291851,2.43872890209282,
95.5054733139421));
#11988=CARTESIAN_POINT('Ctrl Pts',(-0.333939373021536,2.42763974780979,
95.5096898293174));
#11989=CARTESIAN_POINT('Ctrl Pts',(-0.414527398361621,2.41655428314009,
95.5139049417622));
#11990=CARTESIAN_POINT('Ctrl Pts',(-0.494593037235437,2.40144755502427,
95.5181200542071));
#11991=CARTESIAN_POINT('Ctrl Pts',(-0.573709388084008,2.38239538868431,
95.5223351666519));
#11992=CARTESIAN_POINT('Ctrl Pts',(-0.652823684959744,2.36334371696565,
95.5265501696665));
#11993=CARTESIAN_POINT('Ctrl Pts',(-0.730988290805646,2.3403469206185,95.530765172681));
#11994=CARTESIAN_POINT('Ctrl Pts',(-0.807788506305003,2.3135314951566,95.5349801756956));
#11995=CARTESIAN_POINT('Ctrl Pts',(-0.885568922283852,2.28637382465379,
95.5392489747568));
#11996=CARTESIAN_POINT('Ctrl Pts',(-0.961949405885977,2.25529950295276,
95.543517773818));
#11997=CARTESIAN_POINT('Ctrl Pts',(-1.03651886293772,2.22049068828813,95.5477865728792));
#11998=CARTESIAN_POINT('Ctrl Pts',(-1.11025597145398,2.18607041159942,95.5520077233617));
#11999=CARTESIAN_POINT('Ctrl Pts',(-1.18222189460279,2.14799887143268,95.5562288738441));
#12000=CARTESIAN_POINT('Ctrl Pts',(-1.25204455727057,2.10649820237501,95.5604500243266));
#12001=CARTESIAN_POINT('Ctrl Pts',(-1.32304946302162,2.06429484056588,95.5647426476771));
#12002=CARTESIAN_POINT('Ctrl Pts',(-1.39183743708825,2.01854542708319,95.5690352710277));
#12003=CARTESIAN_POINT('Ctrl Pts',(-1.45805013883951,1.96952787302695,95.5733278943783));
#12004=CARTESIAN_POINT('Ctrl Pts',(-1.52426284059078,1.92051031897071,95.5776205177289));
#12005=CARTESIAN_POINT('Ctrl Pts',(-1.58789992707878,1.86822499233759,95.5819131410795));
#12006=CARTESIAN_POINT('Ctrl Pts',(-1.64864180721736,1.81298936607336,95.58620576443));
#12007=CARTESIAN_POINT('Ctrl Pts',(-1.70760629626205,1.75937001032896,95.5903727797077));
#12008=CARTESIAN_POINT('Ctrl Pts',(-1.76407935781339,1.70275513819415,95.5945397949853));
#12009=CARTESIAN_POINT('Ctrl Pts',(-1.81773405989184,1.64340899885242,95.5987068102629));
#12010=CARTESIAN_POINT('Ctrl Pts',(-1.87129837357761,1.58416283587697,95.602866805656));
#12011=CARTESIAN_POINT('Ctrl Pts',(-1.92205344084515,1.52219489923289,95.607026801049));
#12012=CARTESIAN_POINT('Ctrl Pts',(-1.9697069062043,1.45780827053872,95.6111867964421));
#12013=CARTESIAN_POINT('Ctrl Pts',(-2.01731526164687,1.39348259177603,95.6153428538835));
#12014=CARTESIAN_POINT('Ctrl Pts',(-2.0618275538357,1.32674314536301,95.6194989113249));
#12015=CARTESIAN_POINT('Ctrl Pts',(-2.10299044589106,1.25792743609913,95.6236549687662));
#12016=CARTESIAN_POINT('Ctrl Pts',(-2.14412787968735,1.1891542876969,95.627808455786));
#12017=CARTESIAN_POINT('Ctrl Pts',(-2.18191977756558,1.11830783541453,95.6319619428058));
#12018=CARTESIAN_POINT('Ctrl Pts',(-2.21615600002487,1.04575467178195,95.6361154298256));
#12019=CARTESIAN_POINT('Ctrl Pts',(-2.25038227886981,0.97322258058748,95.640267710501));
#12020=CARTESIAN_POINT('Ctrl Pts',(-2.28105472888102,0.898985196785917,
95.6444199911764));
#12021=CARTESIAN_POINT('Ctrl Pts',(-2.30800983772869,0.823432352380932,
95.6485722718519));
#12022=CARTESIAN_POINT('Ctrl Pts',(-2.33497855028516,0.747841377953894,
95.652726648101));
#12023=CARTESIAN_POINT('Ctrl Pts',(-2.35822600958895,0.67093406872749,95.6568810243501));
#12024=CARTESIAN_POINT('Ctrl Pts',(-2.37763779980332,0.593117815401322,
95.6610354005993));
#12025=CARTESIAN_POINT('Ctrl Pts',(-2.39705492978061,0.5152801565098,95.6651909196273));
#12026=CARTESIAN_POINT('Ctrl Pts',(-2.41263419272981,0.436533526438097,
95.6693464386554));
#12027=CARTESIAN_POINT('Ctrl Pts',(-2.42431228652839,0.357295658226464,
95.6735019576834));
#12028=CARTESIAN_POINT('Ctrl Pts',(-2.43600468979453,0.277960697824659,
95.6776625685754));
#12029=CARTESIAN_POINT('Ctrl Pts',(-2.44378633365139,0.198133775714215,
95.6818231794673));
#12030=CARTESIAN_POINT('Ctrl Pts',(-2.44764586026056,0.118237019369414,
95.6859837903593));
#12031=CARTESIAN_POINT('Ctrl Pts',(-2.44958225649275,0.0781513317663674,
95.6880712461721));
#12032=CARTESIAN_POINT('Ctrl Pts',(-2.45053219281933,0.0380480649410048,
95.6901587019849));
#12033=CARTESIAN_POINT('Ctrl Pts',(-2.45049916761641,-0.00201978001007322,
95.6922461577976));
#12034=CARTESIAN_POINT('',(-2.4504995008409,0.00156409031575664,96.4922461578689));
#12035=CARTESIAN_POINT('Ctrl Pts',(-2.45049916761573,-0.00201978082743583,
95.6922461578402));
#12036=CARTESIAN_POINT('Ctrl Pts',(-2.45039286942341,-0.13098606680677,
95.6989650473549));
#12037=CARTESIAN_POINT('Ctrl Pts',(-2.44010274194984,-0.259545593344348,
95.7056839368697));
#12038=CARTESIAN_POINT('Ctrl Pts',(-2.41983633006845,-0.386448425641583,
95.7124028263845));
#12039=CARTESIAN_POINT('Ctrl Pts',(-2.41876093423285,-0.393182265759761,
95.7127593505609));
#12040=CARTESIAN_POINT('Ctrl Pts',(-2.41765745717425,-0.399911448803464,
95.7131158747373));
#12041=CARTESIAN_POINT('Ctrl Pts',(-2.41652593285027,-0.406635790188365,
95.7134723989137));
#12042=CARTESIAN_POINT('Ctrl Pts',(-2.40309990879575,-0.48642300047744,
95.7177027120113));
#12043=CARTESIAN_POINT('Ctrl Pts',(-2.38569278236315,-0.565694995452241,
95.721933025109));
#12044=CARTESIAN_POINT('Ctrl Pts',(-2.36435689547696,-0.644023851119309,
95.7261633382066));
#12045=CARTESIAN_POINT('Ctrl Pts',(-2.34305171746302,-0.722239967586223,
95.7303875625888));
#12046=CARTESIAN_POINT('Ctrl Pts',(-2.31782913063727,-0.799515195737968,
95.7346117869709));
#12047=CARTESIAN_POINT('Ctrl Pts',(-2.28879279169395,-0.875430069560003,
95.7388360113531));
#12048=CARTESIAN_POINT('Ctrl Pts',(-2.25960705229607,-0.951735547606572,
95.7430819706049));
#12049=CARTESIAN_POINT('Ctrl Pts',(-2.22656827742702,-1.02666616172602,
95.7473279298568));
#12050=CARTESIAN_POINT('Ctrl Pts',(-2.1898330725585,-1.09980969459675,95.7515738891086));
#12051=CARTESIAN_POINT('Ctrl Pts',(-2.15335207173773,-1.17244708132813,
95.7557904667351));
#12052=CARTESIAN_POINT('Ctrl Pts',(-2.11322584874696,-1.24332162042607,
95.7600070443615));
#12053=CARTESIAN_POINT('Ctrl Pts',(-2.06965594912513,-1.31204973314693,
95.7642236219879));
#12054=CARTESIAN_POINT('Ctrl Pts',(-2.02610055385468,-1.38075496638667,
95.7684387959223));
#12055=CARTESIAN_POINT('Ctrl Pts',(-1.97910400733192,-1.44731479963216,
95.7726539698566));
#12056=CARTESIAN_POINT('Ctrl Pts',(-1.92891259328625,-1.5113723755123,95.776869143791));
#12057=CARTESIAN_POINT('Ctrl Pts',(-1.87872249225802,-1.57542827563344,
95.7810842074555));
#12058=CARTESIAN_POINT('Ctrl Pts',(-1.82533797761367,-1.63698168303703,
95.7852992711201));
#12059=CARTESIAN_POINT('Ctrl Pts',(-1.76904635879676,-1.69570788475726,
95.7895143347847));
#12060=CARTESIAN_POINT('Ctrl Pts',(-1.7120381014728,-1.755181719223,95.793783059669));
#12061=CARTESIAN_POINT('Ctrl Pts',(-1.65204852131537,-1.81175548766543,
95.7980517845534));
#12062=CARTESIAN_POINT('Ctrl Pts',(-1.58941403354977,-1.86513090156027,
95.8023205094378));
#12063=CARTESIAN_POINT('Ctrl Pts',(-1.52747674843449,-1.91791217824163,
95.8065417179074));
#12064=CARTESIAN_POINT('Ctrl Pts',(-1.4629535570336,-1.96756571271323,95.8107629263769));
#12065=CARTESIAN_POINT('Ctrl Pts',(-1.39620106610138,-2.01384528527326,
95.8149841348465));
#12066=CARTESIAN_POINT('Ctrl Pts',(-1.32832146699419,-2.06090628312303,
95.8192766179382));
#12067=CARTESIAN_POINT('Ctrl Pts',(-1.25813701629652,-2.10447806251757,
95.82356910103));
#12068=CARTESIAN_POINT('Ctrl Pts',(-1.18604930007241,-2.14435008984022,
95.8278615841218));
#12069=CARTESIAN_POINT('Ctrl Pts',(-1.11396158384829,-2.18422211716287,
95.8321540672136));
#12070=CARTESIAN_POINT('Ctrl Pts',(-1.03997107915681,-2.22039423329967,
95.8364465503054));
#12071=CARTESIAN_POINT('Ctrl Pts',(-0.964499265121369,-2.25270757480423,
95.8407390333972));
#12072=CARTESIAN_POINT('Ctrl Pts',(-0.890120388998835,-2.28455297372023,
95.8449693553025));
#12073=CARTESIAN_POINT('Ctrl Pts',(-0.814022428920014,-2.31277072852657,
95.8491996772077));
#12074=CARTESIAN_POINT('Ctrl Pts',(-0.736593675473764,-2.33717350816152,
95.8534299991129));
#12075=CARTESIAN_POINT('Ctrl Pts',(-0.659276337203014,-2.3615411737096,
95.8576542338472));
#12076=CARTESIAN_POINT('Ctrl Pts',(-0.580632448559504,-2.38210462784626,
95.8618784685816));
#12077=CARTESIAN_POINT('Ctrl Pts',(-0.501070928541947,-2.39872428064797,
95.8661027033159));
#12078=CARTESIAN_POINT('Ctrl Pts',(-0.421100282328117,-2.41542939606192,
95.8703486601728));
#12079=CARTESIAN_POINT('Ctrl Pts',(-0.340202976699437,-2.42814984239434,
95.8745946170296));
#12080=CARTESIAN_POINT('Ctrl Pts',(-0.258810455535648,-2.43679449238245,
95.8788405738865));
#12081=CARTESIAN_POINT('Ctrl Pts',(-0.177980848947033,-2.44537935555715,
95.8830571655024));
#12082=CARTESIAN_POINT('Ctrl Pts',(-0.0966633236958435,-2.44994457149375,
95.8872737571182));
#12083=CARTESIAN_POINT('Ctrl Pts',(-0.0152895333809833,-2.45045230114136,
95.8914903487341));
#12084=CARTESIAN_POINT('Ctrl Pts',(0.0660571933746435,-2.4509598619266,
95.8957055379822));
#12085=CARTESIAN_POINT('Ctrl Pts',(0.147459683251942,-2.44741261327396,
95.8999207272304));
#12086=CARTESIAN_POINT('Ctrl Pts',(0.22848457369334,-2.43982479895262,95.9041359164785));
#12087=CARTESIAN_POINT('Ctrl Pts',(0.309507369405125,-2.4322371807984,95.9083509967517));
#12088=CARTESIAN_POINT('Ctrl Pts',(0.390152122053498,-2.42060924909943,
95.9125660770249));
#12089=CARTESIAN_POINT('Ctrl Pts',(0.469990329323206,-2.40500713935378,
95.9167811572982));
#12090=CARTESIAN_POINT('Ctrl Pts',(0.550844327114181,-2.38920652220506,
95.9210498665134));
#12091=CARTESIAN_POINT('Ctrl Pts',(0.630870627672605,-2.36932995950173,
95.9253185757286));
#12092=CARTESIAN_POINT('Ctrl Pts',(0.709636418486952,-2.34549918003759,
95.9295872849438));
#12093=CARTESIAN_POINT('Ctrl Pts',(0.787526091712351,-2.32193347205729,
95.9338085129977));
#12094=CARTESIAN_POINT('Ctrl Pts',(0.864182735228015,-2.29450129435288,
95.9380297410515));
#12095=CARTESIAN_POINT('Ctrl Pts',(0.939206411711731,-2.26336951605335,
95.9422509691054));
#12096=CARTESIAN_POINT('Ctrl Pts',(1.01549590867909,-2.23171247367039,95.9465434189013));
#12097=CARTESIAN_POINT('Ctrl Pts',(1.09009637187876,-2.19623005162782,95.9508358686972));
#12098=CARTESIAN_POINT('Ctrl Pts',(1.16261358044973,-2.15714624273689,95.9551283184931));
#12099=CARTESIAN_POINT('Ctrl Pts',(1.23513078902069,-2.11806243384596,95.959420768289));
#12100=CARTESIAN_POINT('Ctrl Pts',(1.30556435121456,-2.07537755338223,95.963713218085));
#12101=CARTESIAN_POINT('Ctrl Pts',(1.3735527561667,-2.02936026274953,95.9680056678809));
#12102=CARTESIAN_POINT('Ctrl Pts',(1.44054749437405,-1.98401552578859,95.9722353824998));
#12103=CARTESIAN_POINT('Ctrl Pts',(1.50542090464869,-1.93526406958689,95.9764650971188));
#12104=CARTESIAN_POINT('Ctrl Pts',(1.56780550832432,-1.88333112809933,95.9806948117378));
#12105=CARTESIAN_POINT('Ctrl Pts',(1.63010029878634,-1.8314729528857,95.9849184369654));
#12106=CARTESIAN_POINT('Ctrl Pts',(1.68991304412632,-1.77644268409849,95.9891420621931));
#12107=CARTESIAN_POINT('Ctrl Pts',(1.74690526492059,-1.71850872717968,95.9933656874208));
#12108=CARTESIAN_POINT('Ctrl Pts',(1.80420087380922,-1.66026636899938,95.9976117963768));
#12109=CARTESIAN_POINT('Ctrl Pts',(1.85864544215238,-1.5990895796545,96.0018579053327));
#12110=CARTESIAN_POINT('Ctrl Pts',(1.90992890972816,-1.53529209266009,96.0061040142887));
#12111=CARTESIAN_POINT('Ctrl Pts',(1.96084850111177,-1.47194727370347,96.0103199954466));
#12112=CARTESIAN_POINT('Ctrl Pts',(2.0086514099609,-1.40601919440417,96.0145359766045));
#12113=CARTESIAN_POINT('Ctrl Pts',(2.05307245712827,-1.33785041607098,96.0187519577623));
#12114=CARTESIAN_POINT('Ctrl Pts',(2.09747873885647,-1.26970429686029,96.0229665375392));
#12115=CARTESIAN_POINT('Ctrl Pts',(2.13850513733498,-1.19931934717004,96.027181117316));
#12116=CARTESIAN_POINT('Ctrl Pts',(2.1759293612013,-1.12706772869339,96.0313956970928));
#12117=CARTESIAN_POINT('Ctrl Pts',(2.21335263338379,-1.05481794754802,96.0356101696945));
#12118=CARTESIAN_POINT('Ctrl Pts',(2.24717370001357,-0.980702005661079,
96.0398246422961));
#12119=CARTESIAN_POINT('Ctrl Pts',(2.27721654987097,-0.905116033994397,
96.0440391148978));
#12120=CARTESIAN_POINT('Ctrl Pts',(2.30765117962308,-0.828544368088942,
96.0483085471867));
#12121=CARTESIAN_POINT('Ctrl Pts',(2.33420813985629,-0.750464502345619,
96.0525779794756));
#12122=CARTESIAN_POINT('Ctrl Pts',(2.35675574199825,-0.671306653146129,
96.0568474117645));
#12123=CARTESIAN_POINT('Ctrl Pts',(2.37904561615414,-0.593053609385728,
96.0610680427583));
#12124=CARTESIAN_POINT('Ctrl Pts',(2.39741727621602,-0.513747573025114,
96.0652886737521));
#12125=CARTESIAN_POINT('Ctrl Pts',(2.41179491259472,-0.433815109905383,
96.0695093047459));
#12126=CARTESIAN_POINT('Ctrl Pts',(2.4264219123778,-0.352496311048758,96.0738031376823));
#12127=CARTESIAN_POINT('Ctrl Pts',(2.43691496711382,-0.27052964985659,96.0780969706188));
#12128=CARTESIAN_POINT('Ctrl Pts',(2.44324939404552,-0.188368385076181,
96.0823908035552));
#12129=CARTESIAN_POINT('Ctrl Pts',(2.44958382097722,-0.106207120295777,
96.0866846364917));
#12130=CARTESIAN_POINT('Ctrl Pts',(2.45175967380902,-0.0238517532380541,
96.0909784694281));
#12131=CARTESIAN_POINT('Ctrl Pts',(2.44980763300449,0.058247843504729,96.0952723023645));
#12132=CARTESIAN_POINT('Ctrl Pts',(2.44788415030091,0.139146333914604,96.0995033170883));
#12133=CARTESIAN_POINT('Ctrl Pts',(2.44194554762611,0.220101762188912,96.103734331812));
#12134=CARTESIAN_POINT('Ctrl Pts',(2.43198272711111,0.300682997579212,96.1079653465357));
#12135=CARTESIAN_POINT('Ctrl Pts',(2.42203424890235,0.381148229599407,96.1121902703629));
#12136=CARTESIAN_POINT('Ctrl Pts',(2.40807311503856,0.461239881027298,96.1164151941901));
#12137=CARTESIAN_POINT('Ctrl Pts',(2.39014222383595,0.540527889971056,96.1206401180173));
#12138=CARTESIAN_POINT('Ctrl Pts',(2.37212280000661,0.620207378380073,96.1248859021352));
#12139=CARTESIAN_POINT('Ctrl Pts',(2.35009431810921,0.699074790646947,96.1291316862532));
#12140=CARTESIAN_POINT('Ctrl Pts',(2.32415305311903,0.776699965029916,96.1333774703711));
#12141=CARTESIAN_POINT('Ctrl Pts',(2.29838602586768,0.853803760256331,96.137594737151));
#12142=CARTESIAN_POINT('Ctrl Pts',(2.2687587642877,0.92968150691831,96.1418120039309));
#12143=CARTESIAN_POINT('Ctrl Pts',(2.23541615742505,1.00392472482903,96.1460292707107));
#12144=CARTESIAN_POINT('Ctrl Pts',(2.2020846907964,1.07814313703621,96.1502451284424));
#12145=CARTESIAN_POINT('Ctrl Pts',(2.16504053434128,1.15072768114341,96.1544609861741));
#12146=CARTESIAN_POINT('Ctrl Pts',(2.1244766657595,1.22128995191289,96.1586768439058));
#12147=CARTESIAN_POINT('Ctrl Pts',(2.08391391824573,1.2918502725453,96.1628925851234));
#12148=CARTESIAN_POINT('Ctrl Pts',(2.03983188467375,1.36038802835168,96.167108326341));
#12149=CARTESIAN_POINT('Ctrl Pts',(1.99246873056694,1.42654078375383,96.1713240675586));
#12150=CARTESIAN_POINT('Ctrl Pts',(1.94451951631013,1.49351209726268,96.1755919733327));
#12151=CARTESIAN_POINT('Ctrl Pts',(1.89320769161054,1.55803857359002,96.1798598791068));
#12152=CARTESIAN_POINT('Ctrl Pts',(1.83882348335499,1.61977728316649,96.184127784881));
#12153=CARTESIAN_POINT('Ctrl Pts',(1.78502596840533,1.68084995955457,96.1883496487649));
#12154=CARTESIAN_POINT('Ctrl Pts',(1.72822241336629,1.73919443460736,96.1925715126487));
#12155=CARTESIAN_POINT('Ctrl Pts',(1.66873075083071,1.79451607160036,96.1967933765326));
#12156=CARTESIAN_POINT('Ctrl Pts',(1.60826590133106,1.8507426807131,96.2010843032519));
#12157=CARTESIAN_POINT('Ctrl Pts',(1.54502459272168,1.90384634459835,96.2053752299711));
#12158=CARTESIAN_POINT('Ctrl Pts',(1.47937379800963,1.95356172560853,96.2096661566904));
#12159=CARTESIAN_POINT('Ctrl Pts',(1.41372300329758,2.0032771066187,96.2139570834096));
#12160=CARTESIAN_POINT('Ctrl Pts',(1.34566317058895,2.0496039797444,96.2182480101289));
#12161=CARTESIAN_POINT('Ctrl Pts',(1.27558828756782,2.09232520670659,96.2225389368481));
#12162=CARTESIAN_POINT('Ctrl Pts',(1.20649747055948,2.13444649677749,96.2267696058122));
#12163=CARTESIAN_POINT('Ctrl Pts',(1.13518812848537,2.17322115194946,96.2310002747762));
#12164=CARTESIAN_POINT('Ctrl Pts',(1.06201801927646,2.20840847144094,96.2352309437403));
#12165=CARTESIAN_POINT('Ctrl Pts',(0.988953036616486,2.24354523584231,96.2394555343257));
#12166=CARTESIAN_POINT('Ctrl Pts',(0.914033011978542,2.27510470098837,96.2436801249111));
#12167=CARTESIAN_POINT('Ctrl Pts',(0.837642911513598,2.30289048866659,96.2479047154965));
#12168=CARTESIAN_POINT('Ctrl Pts',(0.760868049573986,2.33081622773349,96.2521505844896));
#12169=CARTESIAN_POINT('Ctrl Pts',(0.682608666046283,2.35492991716484,96.2563964534828));
#12170=CARTESIAN_POINT('Ctrl Pts',(0.603278783409193,2.37507999012419,96.2606423224759));
#12171=CARTESIAN_POINT('Ctrl Pts',(0.524488924239545,2.39509289519791,96.2648592885031));
#12172=CARTESIAN_POINT('Ctrl Pts',(0.444643551593448,2.41119586310372,96.2690762545303));
#12173=CARTESIAN_POINT('Ctrl Pts',(0.364164608657989,2.42328999251038,96.2732932205575));
#12174=CARTESIAN_POINT('Ctrl Pts',(0.28371231307121,2.43538011743499,96.2775087903069));
#12175=CARTESIAN_POINT('Ctrl Pts',(0.20262732331826,2.44346397071098,96.2817243600562));
#12176=CARTESIAN_POINT('Ctrl Pts',(0.12134068543824,2.44749396078057,96.2859399298056));
#12177=CARTESIAN_POINT('Ctrl Pts',(0.0400560421298898,2.45152385196424,
96.2901553961154));
#12178=CARTESIAN_POINT('Ctrl Pts',(-0.0414297749209072,2.45150005576119,
96.2943708624251));
#12179=CARTESIAN_POINT('Ctrl Pts',(-0.122683145042565,2.44742703587307,
96.2985863287349));
#12180=CARTESIAN_POINT('Ctrl Pts',(-0.204954313683714,2.44330299639517,
96.3028545989513));
#12181=CARTESIAN_POINT('Ctrl Pts',(-0.28698668293458,2.43502758941941,96.3071228691677));
#12182=CARTESIAN_POINT('Ctrl Pts',(-0.368334710253303,2.42265965237022,
96.3113911393841));
#12183=CARTESIAN_POINT('Ctrl Pts',(-0.448793709332226,2.41042688080282,
96.315612762953));
#12184=CARTESIAN_POINT('Ctrl Pts',(-0.528582802708336,2.39419075039301,
96.3198343865219));
#12185=CARTESIAN_POINT('Ctrl Pts',(-0.607282300202502,2.3740594891158,96.3240560100907));
#12186=CARTESIAN_POINT('Ctrl Pts',(-0.687286177751075,2.35359456858387,
96.3283476036309));
#12187=CARTESIAN_POINT('Ctrl Pts',(-0.766163533826442,2.3291043757461,96.3326391971711));
#12188=CARTESIAN_POINT('Ctrl Pts',(-0.843492566232783,2.30075434166928,
96.3369307907112));
#12189=CARTESIAN_POINT('Ctrl Pts',(-0.920821598639124,2.27240430759245,
96.3412223842514));
#12190=CARTESIAN_POINT('Ctrl Pts',(-0.996601875438346,2.24019468810563,
96.3455139777916));
#12191=CARTESIAN_POINT('Ctrl Pts',(-1.07043757630683,2.20433972999408,96.3498055713318));
#12192=CARTESIAN_POINT('Ctrl Pts',(-1.14314574372558,2.16903230734483,96.3540316286176));
#12193=CARTESIAN_POINT('Ctrl Pts',(-1.21424392411789,2.13005630248263,96.3582576859035));
#12194=CARTESIAN_POINT('Ctrl Pts',(-1.28333670844218,2.08758164936483,96.3624837431893));
#12195=CARTESIAN_POINT('Ctrl Pts',(-1.35232977148203,2.04516829971029,96.366703701027));
#12196=CARTESIAN_POINT('Ctrl Pts',(-1.41932279274412,1.99926657190157,96.3709236588646));
#12197=CARTESIAN_POINT('Ctrl Pts',(-1.48394286364748,1.95009328685315,96.3751436167022));
#12198=CARTESIAN_POINT('Ctrl Pts',(-1.5489774061417,1.90060460552929,96.3793906412486));
#12199=CARTESIAN_POINT('Ctrl Pts',(-1.61160801401144,1.84780245084342,96.383637665795));
#12200=CARTESIAN_POINT('Ctrl Pts',(-1.67148228780926,1.79195346243699,96.3878846903414));
#12201=CARTESIAN_POINT('Ctrl Pts',(-1.73086723760558,1.73656090128643,96.3920970059733));
#12202=CARTESIAN_POINT('Ctrl Pts',(-1.78754039387152,1.6781714474271,96.3963093216053));
#12203=CARTESIAN_POINT('Ctrl Pts',(-1.84119080798415,1.6170858538107,96.4005216372372));
#12204=CARTESIAN_POINT('Ctrl Pts',(-1.89482348312035,1.55602045753896,96.4047325601089));
#12205=CARTESIAN_POINT('Ctrl Pts',(-1.94543509325173,1.4922610416411,96.4089434829805));
#12206=CARTESIAN_POINT('Ctrl Pts',(-1.99275291278564,1.4261437790715,96.4131544058522));
#12207=CARTESIAN_POINT('Ctrl Pts',(-2.04006967858883,1.36002798888147,96.4173652349498));
#12208=CARTESIAN_POINT('Ctrl Pts',(-2.08409252918242,1.29155483616462,96.4215760640475));
#12209=CARTESIAN_POINT('Ctrl Pts',(-2.12459113053335,1.2210908148287,96.4257868931452));
#12210=CARTESIAN_POINT('Ctrl Pts',(-2.16569513849314,1.14957343898717,96.4300606692011));
#12211=CARTESIAN_POINT('Ctrl Pts',(-2.20316839932188,1.07600560064285,96.4343344452569));
#12212=CARTESIAN_POINT('Ctrl Pts',(-2.23681857746337,1.00079613384282,96.4386082213128));
#12213=CARTESIAN_POINT('Ctrl Pts',(-2.27002217192328,0.926584799071467,
96.4428252785412));
#12214=CARTESIAN_POINT('Ctrl Pts',(-2.29950344177342,0.850775612650433,
96.4470423357697));
#12215=CARTESIAN_POINT('Ctrl Pts',(-2.32512700126326,0.77377947633453,96.4512593929982));
#12216=CARTESIAN_POINT('Ctrl Pts',(-2.35126751066703,0.695229959191192,
96.4555615284677));
#12217=CARTESIAN_POINT('Ctrl Pts',(-2.37339281243798,0.615445568424357,
96.4598636639372));
#12218=CARTESIAN_POINT('Ctrl Pts',(-2.39141369418015,0.534874558459875,
96.4641657994068));
#12219=CARTESIAN_POINT('Ctrl Pts',(-2.40943457592232,0.454303548495393,
96.4684679348763));
#12220=CARTESIAN_POINT('Ctrl Pts',(-2.42335102008677,0.372946431201083,
96.4727700703458));
#12221=CARTESIAN_POINT('Ctrl Pts',(-2.43312971698948,0.291255953248524,
96.4770722058154));
#12222=CARTESIAN_POINT('Ctrl Pts',(-2.44462644760282,0.195213154495219,
96.4821301898236));
#12223=CARTESIAN_POINT('Ctrl Pts',(-2.45043764111995,0.09848123134268,96.4871881738319));
#12224=CARTESIAN_POINT('Ctrl Pts',(-2.45049950084054,0.00156409086877713,
96.4922461578401));
#12225=CARTESIAN_POINT('',(0.587285094939578,-2.3790852164775,96.7230107090999));
#12226=CARTESIAN_POINT('Ctrl Pts',(-2.4504995008409,0.00156409031575633,
96.492246157869));
#12227=CARTESIAN_POINT('Ctrl Pts',(-2.45055056711173,-0.0784427161471055,
96.496421612754));
#12228=CARTESIAN_POINT('Ctrl Pts',(-2.44667918136308,-0.15860325583324,
96.5005970676391));
#12229=CARTESIAN_POINT('Ctrl Pts',(-2.43886659932268,-0.238495200597942,
96.5047725225241));
#12230=CARTESIAN_POINT('Ctrl Pts',(-2.43106488590343,-0.31827600217378,
96.5089421686462));
#12231=CARTESIAN_POINT('Ctrl Pts',(-2.41933291332766,-0.397788479137657,
96.5131118147683));
#12232=CARTESIAN_POINT('Ctrl Pts',(-2.40370395745537,-0.476610464544575,
96.5172814608903));
#12233=CARTESIAN_POINT('Ctrl Pts',(-2.38808705541766,-0.555371658483321,
96.5214478911722));
#12234=CARTESIAN_POINT('Ctrl Pts',(-2.3685792236406,-0.633442950428641,
96.525614321454));
#12235=CARTESIAN_POINT('Ctrl Pts',(-2.34526538839251,-0.710408690830951,
96.5297807517359));
#12236=CARTESIAN_POINT('Ctrl Pts',(-2.32196196211607,-0.787340068195104,
96.5339453218239));
#12237=CARTESIAN_POINT('Ctrl Pts',(-2.29485604239929,-0.86316641685313,
96.5381098919118));
#12238=CARTESIAN_POINT('Ctrl Pts',(-2.26408296841375,-0.937485233024396,
96.5422744619997));
#12239=CARTESIAN_POINT('Ctrl Pts',(-2.23331364036793,-1.01179500252692,
96.5464385251436));
#12240=CARTESIAN_POINT('Ctrl Pts',(-2.19887822823037,-1.08459716302059,
96.5506025882874));
#12241=CARTESIAN_POINT('Ctrl Pts',(-2.16096037609839,-1.15550876367629,
96.5547666514312));
#12242=CARTESIAN_POINT('Ctrl Pts',(-2.12300937877822,-1.22648235039439,
96.5589343545138));
#12243=CARTESIAN_POINT('Ctrl Pts',(-2.08157008507773,-1.29556165309398,
96.5631020575963));
#12244=CARTESIAN_POINT('Ctrl Pts',(-2.03687197920892,-1.36238863409584,
96.5672697606788));
#12245=CARTESIAN_POINT('Ctrl Pts',(-1.99215559824111,-1.42924293772516,
96.5714391677526));
#12246=CARTESIAN_POINT('Ctrl Pts',(-1.94417803708808,-1.49384270182766,
96.5756085748265));
#12247=CARTESIAN_POINT('Ctrl Pts',(-1.8932104343097,-1.55586133746581,96.5797779819004));
#12248=CARTESIAN_POINT('Ctrl Pts',(-1.84215338914959,-1.61798880879919,
96.5839547058124));
#12249=CARTESIAN_POINT('Ctrl Pts',(-1.78809614139987,-1.67752574799975,
96.5881314297244));
#12250=CARTESIAN_POINT('Ctrl Pts',(-1.73134796928215,-1.73418120715875,
96.5923081536364));
#12251=CARTESIAN_POINT('Ctrl Pts',(-1.67686192616905,-1.7885782330916,96.5963183825239));
#12252=CARTESIAN_POINT('Ctrl Pts',(-1.61989574806037,-1.84031894392783,
96.6003286114115));
#12253=CARTESIAN_POINT('Ctrl Pts',(-1.5607502269691,-1.88918209260407,96.604338840299));
#12254=CARTESIAN_POINT('Ctrl Pts',(-1.49897684234944,-1.94021625412997,
96.6085272455563));
#12255=CARTESIAN_POINT('Ctrl Pts',(-1.43457128275649,-1.98832161640094,
96.6127156508135));
#12256=CARTESIAN_POINT('Ctrl Pts',(-1.3678458339106,-2.03321125922847,96.6169040560708));
#12257=CARTESIAN_POINT('Ctrl Pts',(-1.30121544998754,-2.0780369469908,96.6210864940333));
#12258=CARTESIAN_POINT('Ctrl Pts',(-1.23227212844164,-2.1196557468126,96.6252689319957));
#12259=CARTESIAN_POINT('Ctrl Pts',(-1.16136171467528,-2.15782047855851,
96.6294513699582));
#12260=CARTESIAN_POINT('Ctrl Pts',(-1.09053096525414,-2.19594233411455,
96.6336291091584));
#12261=CARTESIAN_POINT('Ctrl Pts',(-1.01773792972895,-2.23061760584037,
96.6378068483585));
#12262=CARTESIAN_POINT('Ctrl Pts',(-0.943356620376197,-2.26164288445201,
96.6419845875587));
#12263=CARTESIAN_POINT('Ctrl Pts',(-0.869019872293292,-2.29264957605807,
96.6461598239074));
#12264=CARTESIAN_POINT('Ctrl Pts',(-0.793097175745001,-2.32001043058752,
96.6503350602562));
#12265=CARTESIAN_POINT('Ctrl Pts',(-0.715985096995049,-2.34356898573116,
96.6545102966049));
#12266=CARTESIAN_POINT('Ctrl Pts',(-0.638894427529492,-2.36712100011212,
96.6586843737471));
#12267=CARTESIAN_POINT('Ctrl Pts',(-0.560615485706379,-2.38687267232038,
96.6628584508894));
#12268=CARTESIAN_POINT('Ctrl Pts',(-0.481561179585564,-2.40271702044085,
96.6670325280317));
#12269=CARTESIAN_POINT('Ctrl Pts',(-0.402503410156221,-2.41856206269007,
96.671206788037));
#12270=CARTESIAN_POINT('Ctrl Pts',(-0.322670675394702,-2.43049935006043,
96.6753810480424));
#12271=CARTESIAN_POINT('Ctrl Pts',(-0.242485731844522,-2.43847307138132,
96.6795553080478));
#12272=CARTESIAN_POINT('Ctrl Pts',(-0.162222448688313,-2.44645458292015,
96.6837336462488));
#12273=CARTESIAN_POINT('Ctrl Pts',(-0.0816067436711042,-2.45046475337635,
96.6879119844498));
#12274=CARTESIAN_POINT('Ctrl Pts',(-0.00106534483579401,-2.45049976842284,
96.6920903226507));
#12275=CARTESIAN_POINT('Ctrl Pts',(0.0795205022898598,-2.45053480279304,
96.6962709667465));
#12276=CARTESIAN_POINT('Ctrl Pts',(0.160031487260103,-2.44659034078073,
96.7004516108422));
#12277=CARTESIAN_POINT('Ctrl Pts',(0.240044580309798,-2.43871458958688,
96.7046322549379));
#12278=CARTESIAN_POINT('Ctrl Pts',(0.320185460621495,-2.4308262601931,96.7088195758542));
#12279=CARTESIAN_POINT('Ctrl Pts',(0.399826393045886,-2.41899418310751,
96.7130068967705));
#12280=CARTESIAN_POINT('Ctrl Pts',(0.478553795723909,-2.40331781389775,
96.7171942176868));
#12281=CARTESIAN_POINT('Ctrl Pts',(0.515006479975092,-2.3960592772565,96.7191330481578));
#12282=CARTESIAN_POINT('Ctrl Pts',(0.551263515538092,-2.38797726310625,
96.7210718786289));
#12283=CARTESIAN_POINT('Ctrl Pts',(0.587285094939578,-2.3790852164775,96.7230107090999));
#12284=CARTESIAN_POINT('',(-1.51542342753571,-1.92573157144912,96.7230113585667));
#12285=CARTESIAN_POINT('Origin',(0.,0.,96.7230113585667));
#12286=CARTESIAN_POINT('',(-2.45326580686465,0.00155908382959414,96.6079011502643));
#12287=CARTESIAN_POINT('Ctrl Pts',(-1.51542342753571,-1.92573157144912,
96.7230113585667));
#12288=CARTESIAN_POINT('Ctrl Pts',(-2.09575769702644,-1.46904686999497,
96.6846412891326));
#12289=CARTESIAN_POINT('Ctrl Pts',(-2.44856389678248,-0.732572859810942,
96.6462712196984));
#12290=CARTESIAN_POINT('Ctrl Pts',(-2.45326580686465,0.00155908382959414,
96.6079011502643));
#12291=CARTESIAN_POINT('',(-2.45049904460346,-0.0021638848246924,95.8079011502643));
#12292=CARTESIAN_POINT('Ctrl Pts',(-2.45326580686465,0.00155908382959414,
96.6079011502643));
#12293=CARTESIAN_POINT('Ctrl Pts',(-2.45376236076432,0.0790884438376486,
96.6038490082039));
#12294=CARTESIAN_POINT('Ctrl Pts',(-2.41493050276558,0.96797952800282,96.5573746546489));
#12295=CARTESIAN_POINT('Ctrl Pts',(-1.32808179084826,2.5780765389172,96.4684780895995));
#12296=CARTESIAN_POINT('Ctrl Pts',(1.44992071634245,2.50904073301675,96.3412114551158));
#12297=CARTESIAN_POINT('Ctrl Pts',(2.89498768616649,0.137905795112437,96.2139448206323));
#12298=CARTESIAN_POINT('Ctrl Pts',(1.68109423068961,-2.3612860757178,96.0866781861487));
#12299=CARTESIAN_POINT('Ctrl Pts',(-1.07735437651229,-2.69063721300502,
95.9594115516649));
#12300=CARTESIAN_POINT('Ctrl Pts',(-2.36874873876448,-1.12659486130387,
95.8664858730369));
#12301=CARTESIAN_POINT('Ctrl Pts',(-2.45304861271184,-0.157484081137518,
95.8159824059033));
#12302=CARTESIAN_POINT('Ctrl Pts',(-2.45162076832419,-0.00216487534984322,
95.8079011502643));
#12303=CARTESIAN_POINT('',(-2.45049997932286,-0.000318337325309961,95.007901150296));
#12304=CARTESIAN_POINT('Ctrl Pts',(-2.45049904460346,-0.0021638848246924,
95.8079011502643));
#12305=CARTESIAN_POINT('Ctrl Pts',(-2.45057186376826,0.0803004366316179,
95.8036085307824));
#12306=CARTESIAN_POINT('Ctrl Pts',(-2.4464772602671,0.162905211040847,95.7993159113004));
#12307=CARTESIAN_POINT('Ctrl Pts',(-2.43820288991152,0.245187515235034,
95.7950232918185));
#12308=CARTESIAN_POINT('Ctrl Pts',(-2.43019164838499,0.324853203853163,
95.7908671796343));
#12309=CARTESIAN_POINT('Ctrl Pts',(-2.41826252366292,0.404216102305202,
95.7867110674501));
#12310=CARTESIAN_POINT('Ctrl Pts',(-2.40245714836581,0.48285598294523,95.7825549552659));
#12311=CARTESIAN_POINT('Ctrl Pts',(-2.38666006905027,0.561454586805206,
95.7784010245567));
#12312=CARTESIAN_POINT('Ctrl Pts',(-2.3669908693301,0.639330455758143,95.7742470938474));
#12313=CARTESIAN_POINT('Ctrl Pts',(-2.34354268285201,0.716071186161539,
95.7700931631382));
#12314=CARTESIAN_POINT('Ctrl Pts',(-2.32009911712784,0.792796793858927,
95.7659400510121));
#12315=CARTESIAN_POINT('Ctrl Pts',(-2.29287818369623,0.868387248078455,
95.7617869388861));
#12316=CARTESIAN_POINT('Ctrl Pts',(-2.26202308432463,0.942444595709725,
95.75763382676));
#12317=CARTESIAN_POINT('Ctrl Pts',(-2.23116395036688,1.01651162701583,95.7534801715766));
#12318=CARTESIAN_POINT('Ctrl Pts',(-2.19666989485624,1.08904471184014,95.7493265163932));
#12319=CARTESIAN_POINT('Ctrl Pts',(-2.15873188235456,1.15966672372107,95.7451728612098));
#12320=CARTESIAN_POINT('Ctrl Pts',(-2.12075375704251,1.23036340602312,95.7410148142628));
#12321=CARTESIAN_POINT('Ctrl Pts',(-2.07932464005412,1.29914456203895,95.7368567673158));
#12322=CARTESIAN_POINT('Ctrl Pts',(-2.03468055917747,1.36565928111856,95.7326987203687));
#12323=CARTESIAN_POINT('Ctrl Pts',(-1.99000792123275,1.43221654705597,95.7285380136821));
#12324=CARTESIAN_POINT('Ctrl Pts',(-1.94211651827156,1.49650411024708,95.7243773069955));
#12325=CARTESIAN_POINT('Ctrl Pts',(-1.89128306807474,1.55820364728549,95.7202166003089));
#12326=CARTESIAN_POINT('Ctrl Pts',(-1.84036955354491,1.62000036309615,95.7160493403743));
#12327=CARTESIAN_POINT('Ctrl Pts',(-1.786505075931,1.67920057315013,95.7118820804397));
#12328=CARTESIAN_POINT('Ctrl Pts',(-1.73000296549313,1.73552297287734,95.7077148205051));
#12329=CARTESIAN_POINT('Ctrl Pts',(-1.71718316103575,1.74830200264238,95.7067693079026));
#12330=CARTESIAN_POINT('Ctrl Pts',(-1.70422770338532,1.76093305184202,95.7058237953001));
#12331=CARTESIAN_POINT('Ctrl Pts',(-1.69114047383206,1.77341313510616,95.7048782826977));
#12332=CARTESIAN_POINT('Ctrl Pts',(-1.63258678848454,1.82925038206401,95.7006479567));
#12333=CARTESIAN_POINT('Ctrl Pts',(-1.57115433470712,1.8822898302454,95.6964176307023));
#12334=CARTESIAN_POINT('Ctrl Pts',(-1.50714141443661,1.93222022732659,95.6921873047047));
#12335=CARTESIAN_POINT('Ctrl Pts',(-1.44322061737361,1.98207876784644,95.6879630667155));
#12336=CARTESIAN_POINT('Ctrl Pts',(-1.37672709290479,2.02883685983672,95.6837388287262));
#12337=CARTESIAN_POINT('Ctrl Pts',(-1.30799515958366,2.07222076828356,95.679514590737));
#12338=CARTESIAN_POINT('Ctrl Pts',(-1.23890985681637,2.11582772512959,95.6752686347986));
#12339=CARTESIAN_POINT('Ctrl Pts',(-1.16756340468079,2.1560253719669,95.6710226788601));
#12340=CARTESIAN_POINT('Ctrl Pts',(-1.0943281665114,2.19257750466883,95.6667767229217));
#12341=CARTESIAN_POINT('Ctrl Pts',(-1.0215993904063,2.22887685921308,95.6625601301103));
#12342=CARTESIAN_POINT('Ctrl Pts',(-0.947008291469063,2.26158075152008,
95.658343537299));
#12343=CARTESIAN_POINT('Ctrl Pts',(-0.870946059288238,2.29050282947005,
95.6541269444877));
#12344=CARTESIAN_POINT('Ctrl Pts',(-0.79490913810909,2.31941528310657,95.6499117548194));
#12345=CARTESIAN_POINT('Ctrl Pts',(-0.717402490271032,2.34454825625696,
95.6456965651511));
#12346=CARTESIAN_POINT('Ctrl Pts',(-0.638837114124415,2.36576359588552,
95.6414813754828));
#12347=CARTESIAN_POINT('Ctrl Pts',(-0.560273783565406,2.38697838313544,
95.6372662955643));
#12348=CARTESIAN_POINT('Ctrl Pts',(-0.480652228859809,2.40427561942907,
95.6330512156458));
#12349=CARTESIAN_POINT('Ctrl Pts',(-0.400397035619176,2.41756746831756,
95.6288361357274));
#12350=CARTESIAN_POINT('Ctrl Pts',(-0.31912077626077,2.43102842597016,95.6245674284346));
#12351=CARTESIAN_POINT('Ctrl Pts',(-0.237195120187803,2.44038125826275,
95.6202987211419));
#12352=CARTESIAN_POINT('Ctrl Pts',(-0.155068125884885,2.44558870751698,
95.6160300138491));
#12353=CARTESIAN_POINT('Ctrl Pts',(-0.0738546428888111,2.45073823350476,
95.6118087880502));
#12354=CARTESIAN_POINT('Ctrl Pts',(0.00755524985231285,2.45183419442238,
95.6075875622513));
#12355=CARTESIAN_POINT('Ctrl Pts',(0.0887285139580289,2.44889311747385,
95.6033663364524));
#12356=CARTESIAN_POINT('Ctrl Pts',(0.171271366434522,2.44590241747725,95.5990738884127));
#12357=CARTESIAN_POINT('Ctrl Pts',(0.253569030853064,2.43873723534178,95.594781440373));
#12358=CARTESIAN_POINT('Ctrl Pts',(0.335173854290735,2.4274696161641,95.5904889923333));
#12359=CARTESIAN_POINT('Ctrl Pts',(0.4167786777284,2.41620199698643,95.5861965442936));
#12360=CARTESIAN_POINT('Ctrl Pts',(0.497690182935501,2.40083209919264,95.5819040962539));
#12361=CARTESIAN_POINT('Ctrl Pts',(0.577475747145409,2.38148525325244,95.5776116482142));
#12362=CARTESIAN_POINT('Ctrl Pts',(0.65610621664613,2.36241850108116,95.5733813440481));
#12363=CARTESIAN_POINT('Ctrl Pts',(0.733939585817066,2.3394173604224,95.569151039882));
#12364=CARTESIAN_POINT('Ctrl Pts',(0.810552738024953,2.31256448750738,95.5649207357159));
#12365=CARTESIAN_POINT('Ctrl Pts',(0.887055655155746,2.28575025193373,95.5606965183364));
#12366=CARTESIAN_POINT('Ctrl Pts',(0.962341406996425,2.25509544343965,95.5564723009569));
#12367=CARTESIAN_POINT('Ctrl Pts',(1.03599896479609,2.22073330117361,95.5522480835774));
#12368=CARTESIAN_POINT('Ctrl Pts',(1.11003566973322,2.18619428217874,95.5480021223338));
#12369=CARTESIAN_POINT('Ctrl Pts',(1.18242690642223,2.14790976166453,95.5437561610902));
#12370=CARTESIAN_POINT('Ctrl Pts',(1.25277264201465,2.10606527852762,95.5395101998465));
#12371=CARTESIAN_POINT('Ctrl Pts',(1.32263152168892,2.06451039694347,95.5352936244831));
#12372=CARTESIAN_POINT('Ctrl Pts',(1.39047271925249,2.01944491435982,95.5310770491197));
#12373=CARTESIAN_POINT('Ctrl Pts',(1.45592796740956,1.97109715735036,95.5268604737563));
#12374=CARTESIAN_POINT('Ctrl Pts',(1.52136145328513,1.92276547479677,95.5226453003019));
#12375=CARTESIAN_POINT('Ctrl Pts',(1.58441019116937,1.87115396103302,95.5184301268474));
#12376=CARTESIAN_POINT('Ctrl Pts',(1.64473575083004,1.81653366606335,95.514214953393));
#12377=CARTESIAN_POINT('Ctrl Pts',(1.7050597578607,1.76191477688434,95.5099998884267));
#12378=CARTESIAN_POINT('Ctrl Pts',(1.76266038190972,1.7042875734684,95.5057848234603));
#12379=CARTESIAN_POINT('Ctrl Pts',(1.8172341749178,1.64396174028194,95.501569758494));
#12380=CARTESIAN_POINT('Ctrl Pts',(1.87250276982559,1.5828678735543,95.4973010297637));
#12381=CARTESIAN_POINT('Ctrl Pts',(1.92466657495848,1.51900652598195,95.4930323010334));
#12382=CARTESIAN_POINT('Ctrl Pts',(1.97345199368759,1.45273448317663,95.4887635723031));
#12383=CARTESIAN_POINT('Ctrl Pts',(2.02169438905759,1.38720010478492,95.4845423581678));
#12384=CARTESIAN_POINT('Ctrl Pts',(2.06663302539075,1.31930885799789,95.4803211440326));
#12385=CARTESIAN_POINT('Ctrl Pts',(2.10804767972721,1.24943396383991,95.4760999298973));
#12386=CARTESIAN_POINT('Ctrl Pts',(2.15016158804585,1.17837928685443,95.4718074438695));
#12387=CARTESIAN_POINT('Ctrl Pts',(2.18863118070265,1.10527380325279,95.4675149578417));
#12388=CARTESIAN_POINT('Ctrl Pts',(2.2232750313747,1.0305330585992,95.4632224718139));
#12389=CARTESIAN_POINT('Ctrl Pts',(2.25791888204675,0.955792313945615,95.4589299857861));
#12390=CARTESIAN_POINT('Ctrl Pts',(2.28873686598192,0.879416795412588,95.4546374997582));
#12391=CARTESIAN_POINT('Ctrl Pts',(2.31560051147203,0.80183821390008,95.4503450137304));
#12392=CARTESIAN_POINT('Ctrl Pts',(2.34207419472043,0.725385790695685,95.446114838958));
#12393=CARTESIAN_POINT('Ctrl Pts',(2.3648074862182,0.647476656161797,95.4418846641855));
#12394=CARTESIAN_POINT('Ctrl Pts',(2.38364112932792,0.568511404086408,95.4376544894131));
#12395=CARTESIAN_POINT('Ctrl Pts',(2.402447661774,0.489659820958448,95.4334304038951));
#12396=CARTESIAN_POINT('Ctrl Pts',(2.4173655873715,0.409755588227427,95.4292063183771));
#12397=CARTESIAN_POINT('Ctrl Pts',(2.42828473548847,0.329216484085645,95.4249822328591));
#12398=CARTESIAN_POINT('Ctrl Pts',(2.43926051618846,0.248259660772587,95.4207362389586));
#12399=CARTESIAN_POINT('Ctrl Pts',(2.4461957597747,0.16666181039205,95.4164902450581));
#12400=CARTESIAN_POINT('Ctrl Pts',(2.44903022958949,0.0848597935236164,
95.4122442511576));
#12401=CARTESIAN_POINT('Ctrl Pts',(2.45184496926564,0.00362718301291821,
95.4080278127132));
#12402=CARTESIAN_POINT('Ctrl Pts',(2.45061582686108,-0.0778062896216502,
95.4038113742689));
#12403=CARTESIAN_POINT('Ctrl Pts',(2.44533574317124,-0.159007399730754,
95.3995949358245));
#12404=CARTESIAN_POINT('Ctrl Pts',(2.44005741704231,-0.240181480742424,
95.3953799008896));
#12405=CARTESIAN_POINT('Ctrl Pts',(2.43073085748668,-0.32112288897255,95.3911648659547));
#12406=CARTESIAN_POINT('Ctrl Pts',(2.41740107782973,-0.401400397244051,
95.3869498310197));
#12407=CARTESIAN_POINT('Ctrl Pts',(2.40407164574144,-0.481675812311703,
95.3827349059902));
#12408=CARTESIAN_POINT('Ctrl Pts',(2.38673927833838,-0.561286903095675,
95.3785199809606));
#12409=CARTESIAN_POINT('Ctrl Pts',(2.36550040385334,-0.639810979406937,
95.374305055931));
#12410=CARTESIAN_POINT('Ctrl Pts',(2.34398960297419,-0.719340418264053,
95.3700361662074));
#12411=CARTESIAN_POINT('Ctrl Pts',(2.31847166113447,-0.797754333226607,
95.3657672764837));
#12412=CARTESIAN_POINT('Ctrl Pts',(2.28909880358271,-0.874629588703803,
95.36149838676));
#12413=CARTESIAN_POINT('Ctrl Pts',(2.26005496356092,-0.950643732638566,
95.3572773146363));
#12414=CARTESIAN_POINT('Ctrl Pts',(2.22724238417466,-1.02515310930849,95.3530562425126));
#12415=CARTESIAN_POINT('Ctrl Pts',(2.19085594488886,-1.09777068586528,95.3488351703889));
#12416=CARTESIAN_POINT('Ctrl Pts',(2.15385121048255,-1.17162221369981,95.3445423718652));
#12417=CARTESIAN_POINT('Ctrl Pts',(2.11315027673689,-1.24351661304794,95.3402495733416));
#12418=CARTESIAN_POINT('Ctrl Pts',(2.06900468655941,-1.3130764855846,95.3359567748179));
#12419=CARTESIAN_POINT('Ctrl Pts',(2.02485909638192,-1.38263635812126,95.3316639762942));
#12420=CARTESIAN_POINT('Ctrl Pts',(1.97726919235437,-1.44986133527768,95.3273711777705));
#12421=CARTESIAN_POINT('Ctrl Pts',(1.92652876514865,-1.51440984117735,95.3230783792469));
#12422=CARTESIAN_POINT('Ctrl Pts',(1.87652766876007,-1.57801782090804,95.3188481304181));
#12423=CARTESIAN_POINT('Ctrl Pts',(1.82327869572507,-1.63926675901647,95.3146178815893));
#12424=CARTESIAN_POINT('Ctrl Pts',(1.7670327494766,-1.69780608794914,95.3103876327606));
#12425=CARTESIAN_POINT('Ctrl Pts',(1.71086775324413,-1.75626116619479,95.3061634721698));
#12426=CARTESIAN_POINT('Ctrl Pts',(1.65171466970017,-1.81201404765782,95.3019393115791));
#12427=CARTESIAN_POINT('Ctrl Pts',(1.58986539695636,-1.86474616759515,95.2977151509884));
#12428=CARTESIAN_POINT('Ctrl Pts',(1.52769671841289,-1.91775060997361,95.293469175729));
#12429=CARTESIAN_POINT('Ctrl Pts',(1.46280421402332,-1.96770262371319,95.2892232004696));
#12430=CARTESIAN_POINT('Ctrl Pts',(1.3955228091021,-2.01431535248972,95.2849772252102));
#12431=CARTESIAN_POINT('Ctrl Pts',(1.32870822224629,-2.06060466852098,95.2807607097691));
#12432=CARTESIAN_POINT('Ctrl Pts',(1.25953816713321,-2.10360062240015,95.2765441943279));
#12433=CARTESIAN_POINT('Ctrl Pts',(1.18837328327255,-2.14306303911108,95.2723276788867));
#12434=CARTESIAN_POINT('Ctrl Pts',(1.11723207803241,-2.18251232553163,95.2681125664024));
#12435=CARTESIAN_POINT('Ctrl Pts',(1.04409776859277,-2.21843018410425,95.2638974539182));
#12436=CARTESIAN_POINT('Ctrl Pts',(0.96935746782782,-2.25062132522698,95.259682341434));
#12437=CARTESIAN_POINT('Ctrl Pts',(0.894619107899231,-2.28281163041867,
95.2554673384067));
#12438=CARTESIAN_POINT('Ctrl Pts',(0.818275267222027,-2.31127522753333,
95.2512523353794));
#12439=CARTESIAN_POINT('Ctrl Pts',(0.740733675418833,-2.33586469473309,
95.2470373323521));
#12440=CARTESIAN_POINT('Ctrl Pts',(0.662202422950886,-2.36076799645557,
95.2427685333863));
#12441=CARTESIAN_POINT('Ctrl Pts',(0.582443089080039,-2.38169741057815,
95.2384997344206));
#12442=CARTESIAN_POINT('Ctrl Pts',(0.501893893863773,-2.39855222359286,
95.2342309354548));
#12443=CARTESIAN_POINT('Ctrl Pts',(0.422243792575454,-2.41521890238727,
95.2300097850251));
#12444=CARTESIAN_POINT('Ctrl Pts',(0.341821849958334,-2.42790147720855,
95.2257886345954));
#12445=CARTESIAN_POINT('Ctrl Pts',(0.261059029304541,-2.43655462348345,
95.2215674841657));
#12446=CARTESIAN_POINT('Ctrl Pts',(0.178928727119419,-2.44535428541522,
95.217274860932));
#12447=CARTESIAN_POINT('Ctrl Pts',(0.0964463982607014,-2.44998677244189,
95.2129822376982));
#12448=CARTESIAN_POINT('Ctrl Pts',(0.0140654582285057,-2.45045963298415,
95.2086896144645));
#12449=CARTESIAN_POINT('Ctrl Pts',(-0.0683154818036959,-2.45093249352641,
95.2043969912308));
#12450=CARTESIAN_POINT('Ctrl Pts',(-0.15059453789688,-2.44724581645714,
95.200104367997));
#12451=CARTESIAN_POINT('Ctrl Pts',(-0.232325584175832,-2.43946204580792,
95.1958117447633));
#12452=CARTESIAN_POINT('Ctrl Pts',(-0.312868874840373,-2.43179139272798,
95.1915815040338));
#12453=CARTESIAN_POINT('Ctrl Pts',(-0.393183743365405,-2.42011306134111,
95.1873512633044));
#12454=CARTESIAN_POINT('Ctrl Pts',(-0.472839625236135,-2.40444857270987,
95.183121022575));
#12455=CARTESIAN_POINT('Ctrl Pts',(-0.55238086599157,-2.38880662848346,
95.1788968700276));
#12456=CARTESIAN_POINT('Ctrl Pts',(-0.631264551134139,-2.36919000969627,
95.1746727174803));
#12457=CARTESIAN_POINT('Ctrl Pts',(-0.709064872687081,-2.34567202658881,
95.170448564933));
#12458=CARTESIAN_POINT('Ctrl Pts',(-0.787267161494991,-2.32203253422633,
95.1662025876558));
#12459=CARTESIAN_POINT('Ctrl Pts',(-0.86437438491763,-2.29445128838241,
95.1619566103786));
#12460=CARTESIAN_POINT('Ctrl Pts',(-0.939964141988851,-2.26305494006998,
95.1577106331013));
#12461=CARTESIAN_POINT('Ctrl Pts',(-1.01502925989475,-2.23187650162539,
95.1534941255044));
#12462=CARTESIAN_POINT('Ctrl Pts',(-1.08859747379438,-2.19693593212704,
95.1492776179075));
#12463=CARTESIAN_POINT('Ctrl Pts',(-1.16027175212964,-2.15840675295691,
95.1450611103106));
#12464=CARTESIAN_POINT('Ctrl Pts',(-1.23192218389073,-2.11989039273593,
95.1408460055776));
#12465=CARTESIAN_POINT('Ctrl Pts',(-1.30167952198786,-2.07778801388991,
95.1366309008446));
#12466=CARTESIAN_POINT('Ctrl Pts',(-1.36917018009721,-2.03231967660911,
95.1324157961116));
#12467=CARTESIAN_POINT('Ctrl Pts',(-1.43665908729011,-1.98685251891764,
95.1282008007315));
#12468=CARTESIAN_POINT('Ctrl Pts',(-1.50188104620748,-1.93801983720586,
95.1239858053514));
#12469=CARTESIAN_POINT('Ctrl Pts',(-1.5644915911768,-1.88608491620529,95.1197708099713));
#12470=CARTESIAN_POINT('Ctrl Pts',(-1.62790148618433,-1.83348694106412,
95.1155020016636));
#12471=CARTESIAN_POINT('Ctrl Pts',(-1.68863242610859,-1.7777072496585,95.111233193356));
#12472=CARTESIAN_POINT('Ctrl Pts',(-1.74636274837719,-1.71906003416997,
95.1069643850484));
#12473=CARTESIAN_POINT('Ctrl Pts',(-1.80344845827463,-1.66106766901229,
95.1027432419284));
#12474=CARTESIAN_POINT('Ctrl Pts',(-1.85759995945713,-1.60027189105454,
95.0985220988084));
#12475=CARTESIAN_POINT('Ctrl Pts',(-1.90854611158219,-1.53701073189633,
95.0943009556885));
#12476=CARTESIAN_POINT('Ctrl Pts',(-1.96035519034814,-1.47267805433499,
95.090008314787));
#12477=CARTESIAN_POINT('Ctrl Pts',(-2.00884903343694,-1.40579611070822,
95.0857156738855));
#12478=CARTESIAN_POINT('Ctrl Pts',(-2.05378883540593,-1.33675041408707,
95.081423032984));
#12479=CARTESIAN_POINT('Ctrl Pts',(-2.09872863737492,-1.26770471746592,
95.0771303920826));
#12480=CARTESIAN_POINT('Ctrl Pts',(-2.14011420528511,-1.19649573242134,
95.0728377511811));
#12481=CARTESIAN_POINT('Ctrl Pts',(-2.17775685604983,-1.12353252108159,
95.0685451102796));
#12482=CARTESIAN_POINT('Ctrl Pts',(-2.21719928527825,-1.0470807770869,95.0640472287139));
#12483=CARTESIAN_POINT('Ctrl Pts',(-2.25266677780864,-0.96844397721106,
95.0595493471482));
#12484=CARTESIAN_POINT('Ctrl Pts',(-2.28392751385978,-0.888045810436754,
95.0550514655825));
#12485=CARTESIAN_POINT('Ctrl Pts',(-2.31508961490446,-0.807901318869803,
95.0505677758956));
#12486=CARTESIAN_POINT('Ctrl Pts',(-2.34207126954516,-0.726006882702449,
95.0460840862087));
#12487=CARTESIAN_POINT('Ctrl Pts',(-2.36468776859533,-0.642807908364263,
95.0416003965217));
#12488=CARTESIAN_POINT('Ctrl Pts',(-2.38726029594484,-0.559770692058838,
95.0371254241637));
#12489=CARTESIAN_POINT('Ctrl Pts',(-2.40548445807782,-0.475434345746077,
95.0326504518057));
#12490=CARTESIAN_POINT('Ctrl Pts',(-2.41922415952532,-0.390262368117945,
95.0281754794477));
#12491=CARTESIAN_POINT('Ctrl Pts',(-2.43292775069282,-0.305314236981045,
95.0237122680807));
#12492=CARTESIAN_POINT('Ctrl Pts',(-2.44217029994478,-0.219535219633665,
95.0192490567136));
#12493=CARTESIAN_POINT('Ctrl Pts',(-2.44686627099133,-0.133400531801645,
95.0147858453466));
#12494=CARTESIAN_POINT('Ctrl Pts',(-2.44928084993937,-0.0891117144574003,
95.0124909469964));
#12495=CARTESIAN_POINT('Ctrl Pts',(-2.45049421005239,-0.0447290804429846,
95.0101960486462));
#12496=CARTESIAN_POINT('Ctrl Pts',(-2.45049997932286,-0.00031833732531135,
95.007901150296));
#12497=CARTESIAN_POINT('',(-2.45049895420016,0.00226394874618012,94.2079011502221));
#12498=CARTESIAN_POINT('Ctrl Pts',(-2.45049997932294,-0.000318336712990411,
95.0079011502643));
#12499=CARTESIAN_POINT('Ctrl Pts',(-2.45051097724511,0.0843417321286243,
95.0035263922964));
#12500=CARTESIAN_POINT('Ctrl Pts',(-2.44613038789473,0.168935422682587,
94.9991516343285));
#12501=CARTESIAN_POINT('Ctrl Pts',(-2.43740472998465,0.252998877958903,
94.9947768763606));
#12502=CARTESIAN_POINT('Ctrl Pts',(-2.42851264297302,0.338665720106336,
94.9903186763136));
#12503=CARTESIAN_POINT('Ctrl Pts',(-2.41510809386072,0.423781445560833,
94.9858604762665));
#12504=CARTESIAN_POINT('Ctrl Pts',(-2.39729475185905,0.507866244900213,
94.9814022762195));
#12505=CARTESIAN_POINT('Ctrl Pts',(-2.37975433706502,0.590662738570381,
94.9770123825065));
#12506=CARTESIAN_POINT('Ctrl Pts',(-2.35793947976719,0.67245930123738,94.9726224887935));
#12507=CARTESIAN_POINT('Ctrl Pts',(-2.33199926746043,0.752814496781243,
94.9682325950806));
#12508=CARTESIAN_POINT('Ctrl Pts',(-2.30545361425104,0.835045171274418,
94.9637402418665));
#12509=CARTESIAN_POINT('Ctrl Pts',(-2.27458781118937,0.915765926586604,
94.9592478886524));
#12510=CARTESIAN_POINT('Ctrl Pts',(-2.23961263170089,0.994527782380069,
94.9547555354383));
#12511=CARTESIAN_POINT('Ctrl Pts',(-2.20463745221241,1.07328963817353,94.9502631822242));
#12512=CARTESIAN_POINT('Ctrl Pts',(-2.16555316844435,1.15009222325543,94.9457708290101));
#12513=CARTESIAN_POINT('Ctrl Pts',(-2.12261843975362,1.22451672476038,94.941278475796));
#12514=CARTESIAN_POINT('Ctrl Pts',(-2.08218883859461,1.29459875401873,94.9370482394757));
#12515=CARTESIAN_POINT('Ctrl Pts',(-2.03820844252071,1.36280850261209,94.9328180031553));
#12516=CARTESIAN_POINT('Ctrl Pts',(-1.9908756524753,1.42876323664247,94.928587766835));
#12517=CARTESIAN_POINT('Ctrl Pts',(-1.94361098566699,1.49462304599208,94.9243636188393));
#12518=CARTESIAN_POINT('Ctrl Pts',(-1.89300377622801,1.55823391176525,94.9201394708436));
#12519=CARTESIAN_POINT('Ctrl Pts',(-1.83929756082253,1.61923893627601,94.9159153228479));
#12520=CARTESIAN_POINT('Ctrl Pts',(-1.78531379163511,1.68055923482244,94.9116693444506));
#12521=CARTESIAN_POINT('Ctrl Pts',(-1.72819912731434,1.73924626559179,94.9074233660533));
#12522=CARTESIAN_POINT('Ctrl Pts',(-1.66824421339529,1.79496838258314,94.903177387656));
#12523=CARTESIAN_POINT('Ctrl Pts',(-1.60870550769628,1.85030367551598,94.8989608849262));
#12524=CARTESIAN_POINT('Ctrl Pts',(-1.54636620690215,1.90271476844622,94.8947443821964));
#12525=CARTESIAN_POINT('Ctrl Pts',(-1.48154905552329,1.95191256107389,94.8905278794667));
#12526=CARTESIAN_POINT('Ctrl Pts',(-1.41675347098861,2.00109398394286,94.8863127797091));
#12527=CARTESIAN_POINT('Ctrl Pts',(-1.349482043334,2.04706394865548,94.8820976799514));
#12528=CARTESIAN_POINT('Ctrl Pts',(-1.28009011475513,2.08957401115783,94.8778825801938));
#12529=CARTESIAN_POINT('Ctrl Pts',(-1.21069998809592,2.13208296978946,94.8736675898909));
#12530=CARTESIAN_POINT('Ctrl Pts',(-1.1391898672171,2.17113196274648,94.8694525995879));
#12531=CARTESIAN_POINT('Ctrl Pts',(-1.06594231994289,2.20651698850355,94.865237609285));
#12532=CARTESIAN_POINT('Ctrl Pts',(-0.991759431577881,2.24235386650442,
94.8609687952873));
#12533=CARTESIAN_POINT('Ctrl Pts',(-0.915794861525792,2.27443230916632,
94.8566999812896));
#12534=CARTESIAN_POINT('Ctrl Pts',(-0.838468019221021,2.30259020034907,
94.8524311672918));
#12535=CARTESIAN_POINT('Ctrl Pts',(-0.762004800056656,2.33043361074241,
94.8482100294495));
#12536=CARTESIAN_POINT('Ctrl Pts',(-0.684210054419245,2.35444352728177,
94.8439888916072));
#12537=CARTESIAN_POINT('Ctrl Pts',(-0.605503891400048,2.3745136949488,94.8397677537649));
#12538=CARTESIAN_POINT('Ctrl Pts',(-0.525464293866478,2.39492389004507,
94.8354751016895));
#12539=CARTESIAN_POINT('Ctrl Pts',(-0.444482602954371,2.41125950463292,
94.831182449614));
#12540=CARTESIAN_POINT('Ctrl Pts',(-0.363008695972171,2.4234634176419,94.8268897975386));
#12541=CARTESIAN_POINT('Ctrl Pts',(-0.281534788989966,2.43566733065089,
94.8225971454632));
#12542=CARTESIAN_POINT('Ctrl Pts',(-0.199569168688666,2.44373955951889,
94.8183044933878));
#12543=CARTESIAN_POINT('Ctrl Pts',(-0.117562317125274,2.44767835950562,
94.8140118413124));
#12544=CARTESIAN_POINT('Ctrl Pts',(-0.0367478870311017,2.45155988733061,
94.8097816065886));
#12545=CARTESIAN_POINT('Ctrl Pts',(0.044411376960547,2.45144208469561,94.8055513718649));
#12546=CARTESIAN_POINT('Ctrl Pts',(0.125486237175565,2.44728491481468,94.8013211371412));
#12547=CARTESIAN_POINT('Ctrl Pts',(0.206444411099471,2.44313372810454,94.7970969907462));
#12548=CARTESIAN_POINT('Ctrl Pts',(0.287317961892368,2.43495474383967,94.7928728443511));
#12549=CARTESIAN_POINT('Ctrl Pts',(0.367674981959944,2.42275986380012,94.7886486979561));
#12550=CARTESIAN_POINT('Ctrl Pts',(0.448447325408579,2.41050195480795,94.7844027191592));
#12551=CARTESIAN_POINT('Ctrl Pts',(0.528697307574851,2.39418649118031,94.7801567403622));
#12552=CARTESIAN_POINT('Ctrl Pts',(0.607988791770718,2.373878657194,94.7759107615652));
#12553=CARTESIAN_POINT('Ctrl Pts',(0.686729795624061,2.3537118101437,94.7716942604339));
#12554=CARTESIAN_POINT('Ctrl Pts',(0.764525111512021,2.32960796811263,94.7674777593026));
#12555=CARTESIAN_POINT('Ctrl Pts',(0.840957038661839,2.30168232150423,94.7632612581713));
#12556=CARTESIAN_POINT('Ctrl Pts',(0.917363534412393,2.27376596667081,94.7590461600077));
#12557=CARTESIAN_POINT('Ctrl Pts',(0.992407105687038,2.24203049199986,94.7548310618441));
#12558=CARTESIAN_POINT('Ctrl Pts',(1.06568662791332,2.20664049203461,94.7506159636805));
#12559=CARTESIAN_POINT('Ctrl Pts',(1.13896424738483,2.17125141099581,94.7464009749649));
#12560=CARTESIAN_POINT('Ctrl Pts',(1.21047749044841,2.13220819659127,94.7421859862493));
#12561=CARTESIAN_POINT('Ctrl Pts',(1.27984789843215,2.08972237555107,94.7379709975337));
#12562=CARTESIAN_POINT('Ctrl Pts',(1.3501041956662,2.04669399272921,94.7337021816416));
#12563=CARTESIAN_POINT('Ctrl Pts',(1.41816211304461,2.00013469161971,94.7294333657496));
#12564=CARTESIAN_POINT('Ctrl Pts',(1.48365850661328,1.95030963843028,94.7251645498575));
#12565=CARTESIAN_POINT('Ctrl Pts',(1.54842335255914,1.90104109525967,94.7209434135695));
#12566=CARTESIAN_POINT('Ctrl Pts',(1.61068329043891,1.84857973987824,94.7167222772816));
#12567=CARTESIAN_POINT('Ctrl Pts',(1.6701217908313,1.79322152947996,94.7125011409937));
#12568=CARTESIAN_POINT('Ctrl Pts',(1.73056736750939,1.73692537582029,94.7082084852995));
#12569=CARTESIAN_POINT('Ctrl Pts',(1.78809466152267,1.67763365354351,94.7039158296054));
#12570=CARTESIAN_POINT('Ctrl Pts',(1.84241238017381,1.61569392874463,94.6996231739112));
#12571=CARTESIAN_POINT('Ctrl Pts',(1.89673009882495,1.55375420394576,94.6953305182171));
#12572=CARTESIAN_POINT('Ctrl Pts',(1.94783798495381,1.48916690898437,94.6910378625229));
#12573=CARTESIAN_POINT('Ctrl Pts',(1.99549100323293,1.42231005973256,94.6867452068288));
#12574=CARTESIAN_POINT('Ctrl Pts',(2.04245106751192,1.35642542006574,94.6825149734751));
#12575=CARTESIAN_POINT('Ctrl Pts',(2.0862332327142,1.28808833512064,94.6782847401215));
#12576=CARTESIAN_POINT('Ctrl Pts',(2.12657173800282,1.2176382439492,94.6740545067679));
#12577=CARTESIAN_POINT('Ctrl Pts',(2.16685218614249,1.14728954799325,94.669830361773));
#12578=CARTESIAN_POINT('Ctrl Pts',(2.20369858855441,1.07483428588162,94.665606216778));
#12579=CARTESIAN_POINT('Ctrl Pts',(2.23688743295657,1.00064222491406,94.661382071783));
#12580=CARTESIAN_POINT('Ctrl Pts',(2.27024782690328,0.926066673213479,94.6571360926398));
#12581=CARTESIAN_POINT('Ctrl Pts',(2.29991246275672,0.849736701875051,94.6528901134965));
#12582=CARTESIAN_POINT('Ctrl Pts',(2.32570036411272,0.772054445208349,94.6486441343533));
#12583=CARTESIAN_POINT('Ctrl Pts',(2.35130922224575,0.694911529894342,94.6444276346849));
#12584=CARTESIAN_POINT('Ctrl Pts',(2.3730948585931,0.616435494702253,94.6402111350166));
#12585=CARTESIAN_POINT('Ctrl Pts',(2.39092833146646,0.537040002039902,94.6359946353482));
#12586=CARTESIAN_POINT('Ctrl Pts',(2.40875587047224,0.457670927245963,94.631779538668));
#12587=CARTESIAN_POINT('Ctrl Pts',(2.42263375553616,0.377383456029156,94.6275644419878));
#12588=CARTESIAN_POINT('Ctrl Pts',(2.43248356752879,0.296604018351767,94.6233493453075));
#12589=CARTESIAN_POINT('Ctrl Pts',(2.44233312372074,0.215826678525057,94.6191343580938));
#12590=CARTESIAN_POINT('Ctrl Pts',(2.44815475958035,0.134557859534711,94.6149193708801));
#12591=CARTESIAN_POINT('Ctrl Pts',(2.4499217916521,0.0532302995309846,94.6107043836664));
#12592=CARTESIAN_POINT('Ctrl Pts',(2.45171139082359,-0.0291359100747253,
94.6064355660563));
#12593=CARTESIAN_POINT('Ctrl Pts',(2.44934205773973,-0.11156188344375,94.6021667484462));
#12594=CARTESIAN_POINT('Ctrl Pts',(2.44284051241173,-0.193598762702708,
94.5978979308361));
#12595=CARTESIAN_POINT('Ctrl Pts',(2.4364115895914,-0.274719286911727,94.5936767960804));
#12596=CARTESIAN_POINT('Ctrl Pts',(2.42594243090056,-0.355458907110871,
94.5894556613248));
#12597=CARTESIAN_POINT('Ctrl Pts',(2.41151086214071,-0.435391331766468,
94.5852345265692));
#12598=CARTESIAN_POINT('Ctrl Pts',(2.39683476018089,-0.516678157451295,
94.5809418675318));
#12599=CARTESIAN_POINT('Ctrl Pts',(2.37806083589897,-0.597129689449561,
94.5766492084945));
#12600=CARTESIAN_POINT('Ctrl Pts',(2.35532397543982,-0.676312960631674,
94.5723565494571));
#12601=CARTESIAN_POINT('Ctrl Pts',(2.33258711498066,-0.755496231813789,
94.5680638904198));
#12602=CARTESIAN_POINT('Ctrl Pts',(2.30588754301694,-0.833410792077988,
94.5637712313825));
#12603=CARTESIAN_POINT('Ctrl Pts',(2.27541077160263,-0.909646123761728,
94.5594785723451));
#12604=CARTESIAN_POINT('Ctrl Pts',(2.24537719852325,-0.984772828432255,
94.5552483378774));
#12605=CARTESIAN_POINT('Ctrl Pts',(2.21156232884268,-1.05855218561544,94.5510181034096));
#12606=CARTESIAN_POINT('Ctrl Pts',(2.17410801651075,-1.13057710154755,94.5467878689419));
#12607=CARTESIAN_POINT('Ctrl Pts',(2.13670761009236,-1.20249835601457,94.5425637228159));
#12608=CARTESIAN_POINT('Ctrl Pts',(2.09567837676965,-1.27266977491542,94.5383395766899));
#12609=CARTESIAN_POINT('Ctrl Pts',(2.05121052643643,-1.34070340725918,94.5341154305639));
#12610=CARTESIAN_POINT('Ctrl Pts',(2.00651284152022,-1.40908867525436,94.5298694517013));
#12611=CARTESIAN_POINT('Ctrl Pts',(1.95834106475029,-1.47531355037406,94.5256234728387));
#12612=CARTESIAN_POINT('Ctrl Pts',(1.90693563212919,-1.53900836414753,94.5213774939761));
#12613=CARTESIAN_POINT('Ctrl Pts',(1.85588708562321,-1.60226097184507,94.5171609931438));
#12614=CARTESIAN_POINT('Ctrl Pts',(1.80164993688566,-1.66301817046702,94.5129444923115));
#12615=CARTESIAN_POINT('Ctrl Pts',(1.74450245407991,-1.72094783119918,94.5087279914792));
#12616=CARTESIAN_POINT('Ctrl Pts',(1.68737398625447,-1.77885821669289,94.5045128936253));
#12617=CARTESIAN_POINT('Ctrl Pts',(1.62733743378636,-1.8339426016844,94.5002977957713));
#12618=CARTESIAN_POINT('Ctrl Pts',(1.56470912183818,-1.88590445517168,94.4960826979174));
#12619=CARTESIAN_POINT('Ctrl Pts',(1.50208243623128,-1.93786495930586,94.4918677095217));
#12620=CARTESIAN_POINT('Ctrl Pts',(1.4368644836448,-1.98670279694,94.487652721126));
#12621=CARTESIAN_POINT('Ctrl Pts',(1.36940486835244,-2.03216154784324,94.4834377327304));
#12622=CARTESIAN_POINT('Ctrl Pts',(1.30108375469578,-2.07820083332819,94.4791689164913));
#12623=CARTESIAN_POINT('Ctrl Pts',(1.23046371229256,-2.12077382519476,94.4749001002522));
#12624=CARTESIAN_POINT('Ctrl Pts',(1.15793677929927,-2.15966031244407,94.4706312840131));
#12625=CARTESIAN_POINT('Ctrl Pts',(1.08621993164186,-2.19811245934857,94.4664101480674));
#12626=CARTESIAN_POINT('Ctrl Pts',(1.01263903125177,-2.23295989853074,94.4621890121216));
#12627=CARTESIAN_POINT('Ctrl Pts',(0.937594765481311,-2.26403761137973,
94.4579678761758));
#12628=CARTESIAN_POINT('Ctrl Pts',(0.861278993895383,-2.29564188668107,
94.4536752197901));
#12629=CARTESIAN_POINT('Ctrl Pts',(0.78345028172949,-2.32334733793639,94.4493825634043));
#12630=CARTESIAN_POINT('Ctrl Pts',(0.704545782304668,-2.34703333820308,
94.4450899070186));
#12631=CARTESIAN_POINT('Ctrl Pts',(0.625641282879849,-2.37071933846978,
94.4407972506329));
#12632=CARTESIAN_POINT('Ctrl Pts',(0.545661496307845,-2.39038583338739,
94.4365045942472));
#12633=CARTESIAN_POINT('Ctrl Pts',(0.465052063249206,-2.40596692173181,
94.4322119378615));
#12634=CARTESIAN_POINT('Ctrl Pts',(0.385614821956653,-2.42132143580607,
94.4279817036549));
#12635=CARTESIAN_POINT('Ctrl Pts',(0.305266531096374,-2.43276653384473,
94.4237514694483));
#12636=CARTESIAN_POINT('Ctrl Pts',(0.224426346893148,-2.44020143939393,
94.4195212352417));
#12637=CARTESIAN_POINT('Ctrl Pts',(0.143702511522455,-2.44762564429233,
94.4152970893786));
#12638=CARTESIAN_POINT('Ctrl Pts',(0.0624886481135967,-2.45105107717047,
94.4110729435155));
#12639=CARTESIAN_POINT('Ctrl Pts',(-0.0187860453897214,-2.45042799006594,
94.4068487976525));
#12640=CARTESIAN_POINT('Ctrl Pts',(-0.100480818058492,-2.44980168245206,
94.4026028187244));
#12641=CARTESIAN_POINT('Ctrl Pts',(-0.182236584348602,-2.44508478899653,
94.3983568397963));
#12642=CARTESIAN_POINT('Ctrl Pts',(-0.263612369664805,-2.4362796983433,
94.3941108608681));
#12643=CARTESIAN_POINT('Ctrl Pts',(-0.344423191089381,-2.42753573838469,
94.3898943603011));
#12644=CARTESIAN_POINT('Ctrl Pts',(-0.424858822406461,-2.4147602180408,
94.385677859734));
#12645=CARTESIAN_POINT('Ctrl Pts',(-0.504489413384243,-2.39800764839965,
94.3814613591669));
#12646=CARTESIAN_POINT('Ctrl Pts',(-0.584093508453117,-2.38126065292986,
94.3772462615784));
#12647=CARTESIAN_POINT('Ctrl Pts',(-0.662892640253776,-2.36053933167851,
94.37303116399));
#12648=CARTESIAN_POINT('Ctrl Pts',(-0.740466327717361,-2.33594945739773,
94.3688160664015));
#12649=CARTESIAN_POINT('Ctrl Pts',(-0.818038000737844,-2.31136022166985,
94.3646010782712));
#12650=CARTESIAN_POINT('Ctrl Pts',(-0.894383849573194,-2.28290277422771,
94.3603860901409));
#12651=CARTESIAN_POINT('Ctrl Pts',(-0.969099142057992,-2.25073257026739,
94.3561711020106));
#12652=CARTESIAN_POINT('Ctrl Pts',(-1.04476860243158,-2.2181515297223,94.3519022854579));
#12653=CARTESIAN_POINT('Ctrl Pts',(-1.11876510782296,-2.18176240673814,
94.3476334689051));
#12654=CARTESIAN_POINT('Ctrl Pts',(-1.1906914429175,-2.14177593080206,94.3433646523524));
#12655=CARTESIAN_POINT('Ctrl Pts',(-1.26181439137251,-2.10223608683307,
94.339143516669));
#12656=CARTESIAN_POINT('Ctrl Pts',(-1.33091281827869,-2.05917915330359,
94.3349223809856));
#12657=CARTESIAN_POINT('Ctrl Pts',(-1.39763126139181,-2.01285297704038,
94.3307012453022));
#12658=CARTESIAN_POINT('Ctrl Pts',(-1.46548015621508,-1.96574186781505,
94.3264085883148));
#12659=CARTESIAN_POINT('Ctrl Pts',(-1.53086727006343,-1.91525000978067,
94.3221159313274));
#12660=CARTESIAN_POINT('Ctrl Pts',(-1.59345476753618,-1.86167992786521,
94.3178232743401));
#12661=CARTESIAN_POINT('Ctrl Pts',(-1.65604226500892,-1.80810984594975,
94.3135306173527));
#12662=CARTESIAN_POINT('Ctrl Pts',(-1.71582982997526,-1.75146193146986,
94.3092379603653));
#12663=CARTESIAN_POINT('Ctrl Pts',(-1.77252107491581,-1.69207543832399,
94.3049453033779));
#12664=CARTESIAN_POINT('Ctrl Pts',(-1.827670026992,-1.63430456262863,94.3007694286952));
#12665=CARTESIAN_POINT('Ctrl Pts',(-1.88010845724103,-1.57371206786479,
94.2965935540125));
#12666=CARTESIAN_POINT('Ctrl Pts',(-1.92952846367659,-1.51058603126796,
94.2924176793298));
#12667=CARTESIAN_POINT('Ctrl Pts',(-1.97888391947616,-1.44754244763103,
94.2882472590245));
#12668=CARTESIAN_POINT('Ctrl Pts',(-2.02522847865214,-1.38197225707019,
94.2840768387192));
#12669=CARTESIAN_POINT('Ctrl Pts',(-2.06829116509759,-1.31420010134654,
94.2799064184139));
#12670=CARTESIAN_POINT('Ctrl Pts',(-2.11131161439484,-1.24649441854461,
94.2757400885794));
#12671=CARTESIAN_POINT('Ctrl Pts',(-2.15105632215474,-1.17659145616965,
94.2715737587449));
#12672=CARTESIAN_POINT('Ctrl Pts',(-2.18729570921974,-1.10484737879442,
94.2674074289104));
#12673=CARTESIAN_POINT('Ctrl Pts',(-2.2235113347469,-1.03315034276697,94.2632438308662));
#12674=CARTESIAN_POINT('Ctrl Pts',(-2.25622598685222,-0.95961501333814,
94.2590802328219));
#12675=CARTESIAN_POINT('Ctrl Pts',(-2.2852552468919,-0.884623482931036,
94.2549166347776));
#12676=CARTESIAN_POINT('Ctrl Pts',(-2.31428442192048,-0.809632172133815,
94.2507530489263));
#12677=CARTESIAN_POINT('Ctrl Pts',(-2.33962803644342,-0.73318510766179,
94.246589463075));
#12678=CARTESIAN_POINT('Ctrl Pts',(-2.3611496936317,-0.655684660689062,
94.2424258772237));
#12679=CARTESIAN_POINT('Ctrl Pts',(-2.38267036229203,-0.578187773449548,
94.2382624826132));
#12680=CARTESIAN_POINT('Ctrl Pts',(-2.40036930237333,-0.499638062877898,
94.2340990880028));
#12681=CARTESIAN_POINT('Ctrl Pts',(-2.41416049745554,-0.420451355718133,
94.2299356933924));
#12682=CARTESIAN_POINT('Ctrl Pts',(-2.42796383302171,-0.341194939955018,
94.225768633717));
#12683=CARTESIAN_POINT('Ctrl Pts',(-2.43785248025489,-0.261300880884543,
94.2216015740417));
#12684=CARTESIAN_POINT('Ctrl Pts',(-2.44379203160573,-0.181192594386007,
94.2174345143663));
#12685=CARTESIAN_POINT('Ctrl Pts',(-2.44832151682569,-0.120102239532874,
94.2142567263323));
#12686=CARTESIAN_POINT('Ctrl Pts',(-2.45055545031336,-0.0588874867866859,
94.2110789382982));
#12687=CARTESIAN_POINT('Ctrl Pts',(-2.45049895420091,0.00226394793686294,
94.2079011502642));
#12688=CARTESIAN_POINT('',(-2.45049989228455,-0.000726576496363649,93.4079011502229));
#12689=CARTESIAN_POINT('Ctrl Pts',(-2.45049895420016,0.00226394874617963,
94.2079011502221));
#12690=CARTESIAN_POINT('Ctrl Pts',(-2.45039932002466,0.110108016892512,
94.2022969384674));
#12691=CARTESIAN_POINT('Ctrl Pts',(-2.44317684723875,0.21763439582928,94.1966927267126));
#12692=CARTESIAN_POINT('Ctrl Pts',(-2.4289785155877,0.324058051610146,94.1910885149578));
#12693=CARTESIAN_POINT('Ctrl Pts',(-2.41765385179736,0.408942117617231,
94.1866185662699));
#12694=CARTESIAN_POINT('Ctrl Pts',(-2.40189228346313,0.493125392929466,
94.1821486175821));
#12695=CARTESIAN_POINT('Ctrl Pts',(-2.38178925889044,0.576220596849957,
94.1776786688942));
#12696=CARTESIAN_POINT('Ctrl Pts',(-2.36276431963936,0.654859569852625,
94.1734484346857));
#12697=CARTESIAN_POINT('Ctrl Pts',(-2.33980471071961,0.732703609166421,
94.1692182004772));
#12698=CARTESIAN_POINT('Ctrl Pts',(-2.31299284592925,0.809329564936388,
94.1649879662687));
#12699=CARTESIAN_POINT('Ctrl Pts',(-2.28621956998838,0.885845237162166,
94.1607638204048));
#12700=CARTESIAN_POINT('Ctrl Pts',(-2.2556052017702,0.961145872269699,94.1565396745409));
#12701=CARTESIAN_POINT('Ctrl Pts',(-2.22128274485659,1.0348203792941,94.1523155286769));
#12702=CARTESIAN_POINT('Ctrl Pts',(-2.18678288772607,1.10887568287859,94.1480695497491));
#12703=CARTESIAN_POINT('Ctrl Pts',(-2.14853660786142,1.18128753600972,94.1438235708214));
#12704=CARTESIAN_POINT('Ctrl Pts',(-2.10672922721516,1.25165578862458,94.1395775918936));
#12705=CARTESIAN_POINT('Ctrl Pts',(-2.06521210074575,1.32153549881167,94.1353610913283));
#12706=CARTESIAN_POINT('Ctrl Pts',(-2.02018340462462,1.38939948945081,94.1311445907629));
#12707=CARTESIAN_POINT('Ctrl Pts',(-1.97187125486046,1.45487937790561,94.1269280901976));
#12708=CARTESIAN_POINT('Ctrl Pts',(-1.9235751802654,1.52033747887457,94.1227129926118));
#12709=CARTESIAN_POINT('Ctrl Pts',(-1.87199809752437,1.58341267892187,94.1184978950261));
#12710=CARTESIAN_POINT('Ctrl Pts',(-1.81741086265896,1.64376640867527,94.1142827974403));
#12711=CARTESIAN_POINT('Ctrl Pts',(-1.76282504533444,1.70411857114139,94.1100678093137));
#12712=CARTESIAN_POINT('Ctrl Pts',(-1.70522954413322,1.76174905953555,94.1058528211871));
#12713=CARTESIAN_POINT('Ctrl Pts',(-1.64493386883337,1.81635426532516,94.1016378330605));
#12714=CARTESIAN_POINT('Ctrl Pts',(-1.58386817442722,1.87165681883584,94.0973690165063));
#12715=CARTESIAN_POINT('Ctrl Pts',(-1.52003319995502,1.92385592937759,94.0931001999522));
#12716=CARTESIAN_POINT('Ctrl Pts',(-1.45378561469973,1.97267778324088,94.088831383398));
#12717=CARTESIAN_POINT('Ctrl Pts',(-1.38827798697457,2.02095431762932,94.0846102477207));
#12718=CARTESIAN_POINT('Ctrl Pts',(-1.32041180261381,2.06592845635766,94.0803891120434));
#12719=CARTESIAN_POINT('Ctrl Pts',(-1.25056015427761,2.10737978317463,94.0761679763661));
#12720=CARTESIAN_POINT('Ctrl Pts',(-1.17952496621542,2.14953344548621,94.0718753193735));
#12721=CARTESIAN_POINT('Ctrl Pts',(-1.10643685289585,2.1880435756916,94.0675826623809));
#12722=CARTESIAN_POINT('Ctrl Pts',(-1.03171132518651,2.22272850152282,94.0632900053883));
#12723=CARTESIAN_POINT('Ctrl Pts',(-0.95698579747717,2.25741342735405,94.0589973483957));
#12724=CARTESIAN_POINT('Ctrl Pts',(-0.88062334264572,2.28827302376057,94.0547046914031));
#12725=CARTESIAN_POINT('Ctrl Pts',(-0.803055668404255,2.31517857700951,
94.0504120344106));
#12726=CARTESIAN_POINT('Ctrl Pts',(-0.726615965300836,2.34169287594002,
94.0461818002409));
#12727=CARTESIAN_POINT('Ctrl Pts',(-0.648717580990793,2.3644674163922,94.0419515660712));
#12728=CARTESIAN_POINT('Ctrl Pts',(-0.569761040408466,2.38334273801161,
94.0377213319016));
#12729=CARTESIAN_POINT('Ctrl Pts',(-0.490918137661165,2.40219089341187,
94.0334971860768));
#12730=CARTESIAN_POINT('Ctrl Pts',(-0.411020551847942,2.417150868248,94.0292730402521));
#12731=CARTESIAN_POINT('Ctrl Pts',(-0.330486016570684,2.42811227970439,
94.0250488944273));
#12732=CARTESIAN_POINT('Ctrl Pts',(-0.249535226821358,2.43913034681196,
94.0208029154898));
#12733=CARTESIAN_POINT('Ctrl Pts',(-0.167941333160773,2.44610823691553,
94.0165569365523));
#12734=CARTESIAN_POINT('Ctrl Pts',(-0.0861411529701344,2.4489854943966,
94.0123109576148));
#12735=CARTESIAN_POINT('Ctrl Pts',(-0.00490888407719281,2.45184277604112,
94.0080944570892));
#12736=CARTESIAN_POINT('Ctrl Pts',(0.0765263450380388,2.45065616682677,
94.0038779565636));
#12737=CARTESIAN_POINT('Ctrl Pts',(0.157731302710592,2.44541838672756,93.999661456038));
#12738=CARTESIAN_POINT('Ctrl Pts',(0.238909240605338,2.44018234942409,93.9954463584922));
#12739=CARTESIAN_POINT('Ctrl Pts',(0.319856595358821,2.43089784795572,93.9912312609463));
#12740=CARTESIAN_POINT('Ctrl Pts',(0.400142106332113,2.41760967584515,93.9870161634004));
#12741=CARTESIAN_POINT('Ctrl Pts',(0.480425532421095,2.40432184880683,93.9828011753138));
#12742=CARTESIAN_POINT('Ctrl Pts',(0.560046690133499,2.38703063485041,93.9785861872272));
#12743=CARTESIAN_POINT('Ctrl Pts',(0.63858282950093,2.36583224677207,93.9743711991405));
#12744=CARTESIAN_POINT('Ctrl Pts',(0.718121933438913,2.34436313960355,93.9701023825394));
#12745=CARTESIAN_POINT('Ctrl Pts',(0.796547632615247,2.3188864644694,93.9658335659383));
#12746=CARTESIAN_POINT('Ctrl Pts',(0.873436743013434,2.28955421555247,93.9615647493371));
#12747=CARTESIAN_POINT('Ctrl Pts',(0.94946703299072,2.26054959605185,93.9573436136995));
#12748=CARTESIAN_POINT('Ctrl Pts',(1.02399448335681,2.22777535070441,93.953122478062));
#12749=CARTESIAN_POINT('Ctrl Pts',(1.09663194973094,2.19142616047845,93.9489013424244));
#12750=CARTESIAN_POINT('Ctrl Pts',(1.17050015992039,2.15446108229142,93.9446086853415));
#12751=CARTESIAN_POINT('Ctrl Pts',(1.24241330787115,2.11379903758172,93.9403160282586));
#12752=CARTESIAN_POINT('Ctrl Pts',(1.31199390695758,2.0696913388489,93.9360233711757));
#12753=CARTESIAN_POINT('Ctrl Pts',(1.38157450604402,2.02558364011609,93.9317307140928));
#12754=CARTESIAN_POINT('Ctrl Pts',(1.44882218761369,1.97803062965081,93.9274380570099));
#12755=CARTESIAN_POINT('Ctrl Pts',(1.51339525790319,1.92732587886848,93.923145399927));
#12756=CARTESIAN_POINT('Ctrl Pts',(1.57702932007514,1.87735846599449,93.9189151657679));
#12757=CARTESIAN_POINT('Ctrl Pts',(1.63830607531441,1.82414195352704,93.9146849316088));
#12758=CARTESIAN_POINT('Ctrl Pts',(1.69687482490868,1.76792705692037,93.9104546974497));
#12759=CARTESIAN_POINT('Ctrl Pts',(1.755359279697,1.71179306734748,93.9062305516358));
#12760=CARTESIAN_POINT('Ctrl Pts',(1.81114313664065,1.65266958357601,93.902006405822));
#12761=CARTESIAN_POINT('Ctrl Pts',(1.86390767800933,1.59084833276396,93.8977822600081));
#12762=CARTESIAN_POINT('Ctrl Pts',(1.91694494076326,1.52870754961595,93.8935362810679));
#12763=CARTESIAN_POINT('Ctrl Pts',(1.9669312089842,1.46384132241965,93.8892903021277));
#12764=CARTESIAN_POINT('Ctrl Pts',(2.01357944683973,1.39658442683018,93.8850443231875));
#12765=CARTESIAN_POINT('Ctrl Pts',(2.05990382142216,1.32979447360222,93.8808278226735));
#12766=CARTESIAN_POINT('Ctrl Pts',(2.10293609993088,1.26064732937696,93.8766113221595));
#12767=CARTESIAN_POINT('Ctrl Pts',(2.14243591804438,1.18950350443929,93.8723948216455));
#12768=CARTESIAN_POINT('Ctrl Pts',(2.18192259316115,1.11838335158676,93.8681797241115));
#12769=CARTESIAN_POINT('Ctrl Pts',(2.21787891632128,1.04526824370379,93.8639646265774));
#12770=CARTESIAN_POINT('Ctrl Pts',(2.25010939460911,0.970545188176116,93.8597495290434));
#12771=CARTESIAN_POINT('Ctrl Pts',(2.28233903592208,0.895824073088757,93.8555345409688));
#12772=CARTESIAN_POINT('Ctrl Pts',(2.31084284146848,0.819495520943343,93.8513195528942));
#12773=CARTESIAN_POINT('Ctrl Pts',(2.33547317520619,0.741967181142355,93.8471045648196));
#12774=CARTESIAN_POINT('Ctrl Pts',(2.36041805666823,0.663448746642874,93.8428357482049));
#12775=CARTESIAN_POINT('Ctrl Pts',(2.3813896641976,0.583700122860648,93.8385669315902));
#12776=CARTESIAN_POINT('Ctrl Pts',(2.39828705191424,0.503159484279612,93.8342981149755));
#12777=CARTESIAN_POINT('Ctrl Pts',(2.41499570250767,0.423518452707753,93.8300769793504));
#12778=CARTESIAN_POINT('Ctrl Pts',(2.42772068265479,0.34310348603632,93.8258558437253));
#12779=CARTESIAN_POINT('Ctrl Pts',(2.43641644173113,0.262345521140035,93.8216347081001));
#12780=CARTESIAN_POINT('Ctrl Pts',(2.44525953878754,0.180219220792155,93.8173420509907));
#12781=CARTESIAN_POINT('Ctrl Pts',(2.44993558013904,0.0977386930405679,
93.8130493938812));
#12782=CARTESIAN_POINT('Ctrl Pts',(2.45045187693754,0.0153573699988048,
93.8087567367717));
#12783=CARTESIAN_POINT('Ctrl Pts',(2.45096817373604,-0.0670239530429584,
93.8044640796623));
#12784=CARTESIAN_POINT('Ctrl Pts',(2.44732481460251,-0.149305576184179,
93.8001714225528));
#12785=CARTESIAN_POINT('Ctrl Pts',(2.43958401258297,-0.231041328661296,
93.7958787654433));
#12786=CARTESIAN_POINT('Ctrl Pts',(2.43195577571441,-0.311588496635811,
93.7916485312707));
#12787=CARTESIAN_POINT('Ctrl Pts',(2.42031975512473,-0.391909359454666,
93.7874182970981));
#12788=CARTESIAN_POINT('Ctrl Pts',(2.40469724343616,-0.471573342557164,
93.7831880629255));
#12789=CARTESIAN_POINT('Ctrl Pts',(2.38909721637532,-0.551122669640198,
93.7789639170979));
#12790=CARTESIAN_POINT('Ctrl Pts',(2.36952218193655,-0.630016542030731,
93.7747397712702));
#12791=CARTESIAN_POINT('Ctrl Pts',(2.34604522443331,-0.70782911420317,93.7705156254426));
#12792=CARTESIAN_POINT('Ctrl Pts',(2.32244692287695,-0.786043871918182,
93.7662696465058));
#12793=CARTESIAN_POINT('Ctrl Pts',(2.29490628741051,-0.863165644642283,
93.762023667569));
#12794=CARTESIAN_POINT('Ctrl Pts',(2.26354974573485,-0.93877196303666,93.7577776886322));
#12795=CARTESIAN_POINT('Ctrl Pts',(2.23241090201725,-1.01385337210587,93.7535611881039));
#12796=CARTESIAN_POINT('Ctrl Pts',(2.19750914997221,-1.08743986743532,93.7493446875756));
#12797=CARTESIAN_POINT('Ctrl Pts',(2.15901780038694,-1.15913432681995,93.7451281870473));
#12798=CARTESIAN_POINT('Ctrl Pts',(2.12053925824342,-1.23080493090663,93.7409130894988));
#12799=CARTESIAN_POINT('Ctrl Pts',(2.07847371024361,-1.30058433968162,93.7366979919503));
#12800=CARTESIAN_POINT('Ctrl Pts',(2.03304101838861,-1.36809885152696,93.7324828944018));
#12801=CARTESIAN_POINT('Ctrl Pts',(1.98760950634764,-1.43561161012888,93.7282679063126));
#12802=CARTESIAN_POINT('Ctrl Pts',(1.93881128489416,-1.50085920339646,93.7240529182234));
#12803=CARTESIAN_POINT('Ctrl Pts',(1.88690945597032,-1.56349702748991,93.7198379301341));
#12804=CARTESIAN_POINT('Ctrl Pts',(1.83434480238627,-1.62693478282533,93.7155691135363));
#12805=CARTESIAN_POINT('Ctrl Pts',(1.77859700556951,-1.68769525030285,93.7113002969384));
#12806=CARTESIAN_POINT('Ctrl Pts',(1.71998009048483,-1.74545659881184,93.7070314803405));
#12807=CARTESIAN_POINT('Ctrl Pts',(1.66201790267599,-1.80257277637822,93.7028103447006));
#12808=CARTESIAN_POINT('Ctrl Pts',(1.60125076402844,-1.85675623221234,93.6985892090606));
#12809=CARTESIAN_POINT('Ctrl Pts',(1.53801656220287,-1.90773564845595,93.6943680734207));
#12810=CARTESIAN_POINT('Ctrl Pts',(1.47371094231323,-1.9595788419891,93.6900754163439));
#12811=CARTESIAN_POINT('Ctrl Pts',(1.40685428842817,-2.00810811710232,93.685782759267));
#12812=CARTESIAN_POINT('Ctrl Pts',(1.33783199317452,-2.05308446198365,93.6814901021902));
#12813=CARTESIAN_POINT('Ctrl Pts',(1.26880969792087,-2.09806080686498,93.6771974451134));
#12814=CARTESIAN_POINT('Ctrl Pts',(1.19762222578243,-2.13948402832458,93.6729047880365));
#12815=CARTESIAN_POINT('Ctrl Pts',(1.12467854535163,-2.17716522561466,93.6686121309597));
#12816=CARTESIAN_POINT('Ctrl Pts',(1.05279559644858,-2.21429847092683,93.6643818967915));
#12817=CARTESIAN_POINT('Ctrl Pts',(0.97893608890089,-2.24793789881027,93.6601516626233));
#12818=CARTESIAN_POINT('Ctrl Pts',(0.903473746455619,-2.27786861769186,
93.6559214284551));
#12819=CARTESIAN_POINT('Ctrl Pts',(0.828120012839371,-2.30775625892408,
93.6516972826319));
#12820=CARTESIAN_POINT('Ctrl Pts',(0.751168454586691,-2.3339456220617,93.6474731368088));
#12821=CARTESIAN_POINT('Ctrl Pts',(0.673016820036839,-2.35626794103461,
93.6432489909857));
#12822=CARTESIAN_POINT('Ctrl Pts',(0.594461247347319,-2.37870563617401,
93.6390030120478));
#12823=CARTESIAN_POINT('Ctrl Pts',(0.514693578532129,-2.39723597468178,
93.6347570331099));
#12824=CARTESIAN_POINT('Ctrl Pts',(0.434137563550564,-2.41173688986058,
93.630511054172));
#12825=CARTESIAN_POINT('Ctrl Pts',(0.354140822087412,-2.42613713002641,
93.6262945536483));
#12826=CARTESIAN_POINT('Ctrl Pts',(0.273367110099192,-2.43656363606648,
93.6220780531247));
#12827=CARTESIAN_POINT('Ctrl Pts',(0.192244203631005,-2.44294748534844,
93.617861552601));
#12828=CARTESIAN_POINT('Ctrl Pts',(0.111148289641529,-2.4493292104965,93.6136464550572));
#12829=CARTESIAN_POINT('Ctrl Pts',(0.0297038752827075,-2.45167091359718,
93.6094313575134));
#12830=CARTESIAN_POINT('Ctrl Pts',(-0.0516557960857132,-2.44995549525512,
93.6052162599696));
#12831=CARTESIAN_POINT('Ctrl Pts',(-0.133013354673379,-2.44824012145973,
93.6010012718851));
#12832=CARTESIAN_POINT('Ctrl Pts',(-0.214285709586253,-2.44246784656551,
93.5967862838006));
#12833=CARTESIAN_POINT('Ctrl Pts',(-0.29504071630266,-2.43267367842948,
93.5925712957161));
#12834=CARTESIAN_POINT('Ctrl Pts',(-0.376827024250353,-2.4227544315142,
93.5883024791128));
#12835=CARTESIAN_POINT('Ctrl Pts',(-0.458082188896049,-2.40870987757979,
93.5840336625095));
#12836=CARTESIAN_POINT('Ctrl Pts',(-0.538365689650037,-2.39063017512279,
93.5797648459061));
#12837=CARTESIAN_POINT('Ctrl Pts',(-0.617752455922586,-2.37275241568591,
93.575543710271));
#12838=CARTESIAN_POINT('Ctrl Pts',(-0.696188719385308,-2.35092938689105,
93.5713225746358));
#12839=CARTESIAN_POINT('Ctrl Pts',(-0.773263550488758,-2.32529863275355,
93.5671014390006));
#12840=CARTESIAN_POINT('Ctrl Pts',(-0.851644310689964,-2.29923360004357,
93.5628087819132));
#12841=CARTESIAN_POINT('Ctrl Pts',(-0.928616606842926,-2.26923079398519,
93.5585161248258));
#12842=CARTESIAN_POINT('Ctrl Pts',(-1.00377100109754,-2.23548518835524,
93.5542234677384));
#12843=CARTESIAN_POINT('Ctrl Pts',(-1.07892539535214,-2.20173958272529,
93.549930810651));
#12844=CARTESIAN_POINT('Ctrl Pts',(-1.15226147405417,-2.1642514638063,93.5456381535636));
#12845=CARTESIAN_POINT('Ctrl Pts',(-1.2233992070889,-2.12326273223411,93.5413454964762));
#12846=CARTESIAN_POINT('Ctrl Pts',(-1.29350247020591,-2.08287005015588,
93.5371152623032));
#12847=CARTESIAN_POINT('Ctrl Pts',(-1.36173532530319,-2.03892559130925,
93.5328850281303));
#12848=CARTESIAN_POINT('Ctrl Pts',(-1.42771493428827,-1.99162755464224,
93.5286547939573));
#12849=CARTESIAN_POINT('Ctrl Pts',(-1.49359958242498,-1.94439759145668,
93.5244306481294));
#12850=CARTESIAN_POINT('Ctrl Pts',(-1.55723705026384,-1.89382390501511,
93.5202065023015));
#12851=CARTESIAN_POINT('Ctrl Pts',(-1.61827031211913,-1.84014984360346,
93.5159823564736));
#12852=CARTESIAN_POINT('Ctrl Pts',(-1.67961903321785,-1.78619836004052,
93.5117363775369));
#12853=CARTESIAN_POINT('Ctrl Pts',(-1.73833613527186,-1.72911459391617,
93.5074903986002));
#12854=CARTESIAN_POINT('Ctrl Pts',(-1.79408981881717,-1.66918901626405,
93.5032444196635));
#12855=CARTESIAN_POINT('Ctrl Pts',(-1.84945642322856,-1.60967948180805,
93.4990279191351));
#12856=CARTESIAN_POINT('Ctrl Pts',(-1.90190030582722,-1.54736781541865,
93.4948114186067));
#12857=CARTESIAN_POINT('Ctrl Pts',(-1.95113219657686,-1.48257660897546,
93.4905949180783));
#12858=CARTESIAN_POINT('Ctrl Pts',(-2.00034770612371,-1.41780696087332,
93.4863798205298));
#12859=CARTESIAN_POINT('Ctrl Pts',(-2.04635306492065,-1.3505597811607,93.4821647229812));
#12860=CARTESIAN_POINT('Ctrl Pts',(-2.08889964199823,-1.2811902808169,93.4779496254327));
#12861=CARTESIAN_POINT('Ctrl Pts',(-2.13144511420883,-1.21182258188874,
93.4737346373435));
#12862=CARTESIAN_POINT('Ctrl Pts',(-2.17053174097621,-1.14033306900568,
93.4695196492544));
#12863=CARTESIAN_POINT('Ctrl Pts',(-2.20595531951388,-1.06710420217916,
93.4653046611652));
#12864=CARTESIAN_POINT('Ctrl Pts',(-2.24183128329213,-0.992940148680246,
93.4610358445675));
#12865=CARTESIAN_POINT('Ctrl Pts',(-2.27394974557627,-0.91699243219872,
93.4567670279697));
#12866=CARTESIAN_POINT('Ctrl Pts',(-2.30214836904294,-0.839680377830114,
93.452498211372));
#12867=CARTESIAN_POINT('Ctrl Pts',(-2.33003202526981,-0.763231867896459,
93.4482770757323));
#12868=CARTESIAN_POINT('Ctrl Pts',(-2.35408289289647,-0.685449814745013,
93.4440559400925));
#12869=CARTESIAN_POINT('Ctrl Pts',(-2.37419449592288,-0.606754271125895,
93.4398348044528));
#12870=CARTESIAN_POINT('Ctrl Pts',(-2.3946468628743,-0.526725337906243,
93.4355421473761));
#12871=CARTESIAN_POINT('Ctrl Pts',(-2.41102513613057,-0.445752164087972,
93.4312494902994));
#12872=CARTESIAN_POINT('Ctrl Pts',(-2.42327195772963,-0.364284598742836,
93.4269568332226));
#12873=CARTESIAN_POINT('Ctrl Pts',(-2.43551877932868,-0.282817033397704,
93.4226641761459));
#12874=CARTESIAN_POINT('Ctrl Pts',(-2.44363416644429,-0.200855579290618,
93.4183715190692));
#12875=CARTESIAN_POINT('Ctrl Pts',(-2.44761613749138,-0.118850719357496,
93.4140788619925));
#12876=CARTESIAN_POINT('Ctrl Pts',(-2.44952633505272,-0.0795120396909347,
93.4120196247498));
#12877=CARTESIAN_POINT('Ctrl Pts',(-2.45048821001178,-0.0401269385891838,
93.409960387507));
#12878=CARTESIAN_POINT('Ctrl Pts',(-2.45049989228432,-0.000726577286486693,
93.4079011502642));
#12879=CARTESIAN_POINT('',(-2.45049926108039,-0.00190300932191417,92.6079011502917));
#12880=CARTESIAN_POINT('Ctrl Pts',(-2.45049989228455,-0.000726576496358752,
93.4079011502229));
#12881=CARTESIAN_POINT('Ctrl Pts',(-2.45052370789507,0.0795955249073371,
93.4037031617488));
#12882=CARTESIAN_POINT('Ctrl Pts',(-2.446594086483,0.160078074458993,93.3995051732748));
#12883=CARTESIAN_POINT('Ctrl Pts',(-2.43868984666028,0.240295821428641,
93.3953071848007));
#12884=CARTESIAN_POINT('Ctrl Pts',(-2.43079672481322,0.320400735415266,
93.3911151011492));
#12885=CARTESIAN_POINT('Ctrl Pts',(-2.41894012952624,0.400241119723056,
93.3869230174977));
#12886=CARTESIAN_POINT('Ctrl Pts',(-2.40315089260997,0.479391319641781,
93.3827309338461));
#12887=CARTESIAN_POINT('Ctrl Pts',(-2.38737900061532,0.558454570835878,
93.3785434553166));
#12888=CARTESIAN_POINT('Ctrl Pts',(-2.36768314111001,0.63682868239816,93.3743559767871));
#12889=CARTESIAN_POINT('Ctrl Pts',(-2.34414581799513,0.714094275271782,
93.3701684982576));
#12890=CARTESIAN_POINT('Ctrl Pts',(-2.3206223320979,0.791314444933099,93.3659834814801));
#12891=CARTESIAN_POINT('Ctrl Pts',(-2.2932620011617,0.867426937712915,93.3617984647026));
#12892=CARTESIAN_POINT('Ctrl Pts',(-2.26219786679023,0.942024979228125,
93.357613447925));
#12893=CARTESIAN_POINT('Ctrl Pts',(-2.23114210675983,1.01660291043104,93.353429559354));
#12894=CARTESIAN_POINT('Ctrl Pts',(-2.19638470745337,1.08966676464385,93.349245670783));
#12895=CARTESIAN_POINT('Ctrl Pts',(-2.15810724529095,1.16082874181454,93.3450617822119));
#12896=CARTESIAN_POINT('Ctrl Pts',(-2.1198279183326,1.23199418584424,93.3408776898108));
#12897=CARTESIAN_POINT('Ctrl Pts',(-2.07802841388237,1.30125715337313,93.3366935974097));
#12898=CARTESIAN_POINT('Ctrl Pts',(-2.03293601957873,1.36825487037298,93.3325095050085));
#12899=CARTESIAN_POINT('Ctrl Pts',(-1.98779748611528,1.43532114036097,93.3283211313863));
#12900=CARTESIAN_POINT('Ctrl Pts',(-1.93935960138974,1.50011713980379,93.3241327577642));
#12901=CARTESIAN_POINT('Ctrl Pts',(-1.88789231328252,1.56231010476434,93.319944384142));
#12902=CARTESIAN_POINT('Ctrl Pts',(-1.83639677584122,1.62453720616201,93.3157537116078));
#12903=CARTESIAN_POINT('Ctrl Pts',(-1.78186884546537,1.68415808109405,93.3115630390736));
#12904=CARTESIAN_POINT('Ctrl Pts',(-1.7246162531268,1.74087593740934,93.3073723665395));
#12905=CARTESIAN_POINT('Ctrl Pts',(-1.66726590097464,1.79769064046703,93.3031745383579));
#12906=CARTESIAN_POINT('Ctrl Pts',(-1.60718195106043,1.85159211357102,93.2989767101762));
#12907=CARTESIAN_POINT('Ctrl Pts',(-1.54470580952404,1.90232337209599,93.2947788819946));
#12908=CARTESIAN_POINT('Ctrl Pts',(-1.50518332220491,1.93441603134848,93.2921233304994));
#12909=CARTESIAN_POINT('Ctrl Pts',(-1.46470414331117,1.96524086620808,93.2894677790041));
#12910=CARTESIAN_POINT('Ctrl Pts',(-1.42336023198326,1.99474206352815,93.2868122275088));
#12911=CARTESIAN_POINT('Ctrl Pts',(-1.35750030542381,2.0417368114006,93.282581993338));
#12912=CARTESIAN_POINT('Ctrl Pts',(-1.28918626061932,2.08555494976627,93.2783517591672));
#12913=CARTESIAN_POINT('Ctrl Pts',(-1.21875739691421,2.12593053919146,93.2741215249964));
#12914=CARTESIAN_POINT('Ctrl Pts',(-1.14842989762866,2.16624801823447,93.2698973791708));
#12915=CARTESIAN_POINT('Ctrl Pts',(-1.07599402455916,2.20313255911316,93.2656732333452));
#12916=CARTESIAN_POINT('Ctrl Pts',(-1.0018194275133,2.2363604549931,93.2614490875196));
#12917=CARTESIAN_POINT('Ctrl Pts',(-0.927261448282132,2.2697600940822,93.2572031085823));
#12918=CARTESIAN_POINT('Ctrl Pts',(-0.850947105048476,2.29946489916578,
93.252957129645));
#12919=CARTESIAN_POINT('Ctrl Pts',(-0.773278436698099,2.3252936823846,93.2487111507078));
#12920=CARTESIAN_POINT('Ctrl Pts',(-0.696148995930408,2.35094314500176,
93.2444946501819));
#12921=CARTESIAN_POINT('Ctrl Pts',(-0.617684422978472,2.37277008643907,
93.240278149656));
#12922=CARTESIAN_POINT('Ctrl Pts',(-0.538298312493276,2.39064534734178,
93.2360616491302));
#12923=CARTESIAN_POINT('Ctrl Pts',(-0.458938616594858,2.40851466050845,
93.2318465515842));
#12924=CARTESIAN_POINT('Ctrl Pts',(-0.378658445527426,2.42243480209917,
93.2276314540383));
#12925=CARTESIAN_POINT('Ctrl Pts',(-0.297884188074977,2.43232712859412,
93.2234163564924));
#12926=CARTESIAN_POINT('Ctrl Pts',(-0.217112028203139,2.44221919820089,
93.2192013684059));
#12927=CARTESIAN_POINT('Ctrl Pts',(-0.135846269321706,2.44808360518105,
93.2149863803194));
#12928=CARTESIAN_POINT('Ctrl Pts',(-0.0545196356231395,2.44989343836248,
93.2107713922329));
#12929=CARTESIAN_POINT('Ctrl Pts',(0.0278455993155291,2.4517263844517,93.2065025756323));
#12930=CARTESIAN_POINT('Ctrl Pts',(0.110272786671581,2.44940043248254,93.2022337590317));
#12931=CARTESIAN_POINT('Ctrl Pts',(0.192313055022356,2.44294206621196,93.197964942431));
#12932=CARTESIAN_POINT('Ctrl Pts',(0.273436966586778,2.43655583729393,93.1937438067941));
#12933=CARTESIAN_POINT('Ctrl Pts',(0.354182100494936,2.42612917109596,93.1895226711572));
#12934=CARTESIAN_POINT('Ctrl Pts',(0.434122124168227,2.41173966905793,93.1853015355204));
#12935=CARTESIAN_POINT('Ctrl Pts',(0.51541662363876,2.39710635633097,93.1810088784378));
#12936=CARTESIAN_POINT('Ctrl Pts',(0.595877987104331,2.37837478613998,93.1767162213553));
#12937=CARTESIAN_POINT('Ctrl Pts',(0.675073177205928,2.35567961646254,93.1724235642728));
#12938=CARTESIAN_POINT('Ctrl Pts',(0.754268367307523,2.3329844467851,93.1681309071903));
#12939=CARTESIAN_POINT('Ctrl Pts',(0.83219693382685,2.30632590205602,93.1638382501078));
#12940=CARTESIAN_POINT('Ctrl Pts',(0.908448262154074,2.27588927784048,93.1595455930253));
#12941=CARTESIAN_POINT('Ctrl Pts',(0.983590760481222,2.24589525630179,93.1553153588153));
#12942=CARTESIAN_POINT('Ctrl Pts',(1.05738790226238,2.21211922990983,93.1510851246054));
#12943=CARTESIAN_POINT('Ctrl Pts',(1.12943251915137,2.17470283824788,93.1468548903955));
#12944=CARTESIAN_POINT('Ctrl Pts',(1.20137344616123,2.13734029795328,93.1426307445304));
#12945=CARTESIAN_POINT('Ctrl Pts',(1.27156644837697,2.09634801056346,93.1384065986654));
#12946=CARTESIAN_POINT('Ctrl Pts',(1.33962347476286,2.05191598167768,93.1341824528003));
#12947=CARTESIAN_POINT('Ctrl Pts',(1.40803226298435,2.00725429991298,93.1299364738729));
#12948=CARTESIAN_POINT('Ctrl Pts',(1.47428248740516,1.95911738938175,93.1256904949454));
#12949=CARTESIAN_POINT('Ctrl Pts',(1.53800435297943,1.90774549146796,93.121444516018));
#12950=CARTESIAN_POINT('Ctrl Pts',(1.60128381970143,1.85673025085651,93.1172280154523));
#12951=CARTESIAN_POINT('Ctrl Pts',(1.66206955651884,1.80252509522039,93.1130115148866));
#12952=CARTESIAN_POINT('Ctrl Pts',(1.72002928820667,1.74540811780834,93.1087950143208));
#12953=CARTESIAN_POINT('Ctrl Pts',(1.77796973462824,1.6883101452482,93.104579916735));
#12954=CARTESIAN_POINT('Ctrl Pts',(1.83308571212533,1.62830260114869,93.1003648191491));
#12955=CARTESIAN_POINT('Ctrl Pts',(1.88508052324529,1.56570165449273,93.0961497215633));
#12956=CARTESIAN_POINT('Ctrl Pts',(1.93707398414174,1.50310233348493,93.0919347334369));
#12957=CARTESIAN_POINT('Ctrl Pts',(1.98594614340768,1.43791010235155,93.0877197453105));
#12958=CARTESIAN_POINT('Ctrl Pts',(2.03144039683689,1.37047443029747,93.0835047571841));
#12959=CARTESIAN_POINT('Ctrl Pts',(2.07751564457341,1.3021775562537,93.0792359406306));
#12960=CARTESIAN_POINT('Ctrl Pts',(2.12012580879891,1.23157992872312,93.074967124077));
#12961=CARTESIAN_POINT('Ctrl Pts',(2.15905047210976,1.15907347001069,93.0706983075235));
#12962=CARTESIAN_POINT('Ctrl Pts',(2.19754036337891,1.08737687780473,93.0664771718471));
#12963=CARTESIAN_POINT('Ctrl Pts',(2.2324265290723,1.01381433584631,93.0622560361706));
#12964=CARTESIAN_POINT('Ctrl Pts',(2.26354373970752,0.938786444528733,93.0580349004942));
#12965=CARTESIAN_POINT('Ctrl Pts',(2.2951881885118,0.862487309187705,93.0537422435021));
#12966=CARTESIAN_POINT('Ctrl Pts',(2.32293460907364,0.784673180722974,93.04944958651));
#12967=CARTESIAN_POINT('Ctrl Pts',(2.3466621443104,0.705781149125222,93.0451569295179));
#12968=CARTESIAN_POINT('Ctrl Pts',(2.37038967954715,0.626889117527469,93.0408642725258));
#12969=CARTESIAN_POINT('Ctrl Pts',(2.39009827483509,0.546919682880347,93.0365716155337));
#12970=CARTESIAN_POINT('Ctrl Pts',(2.40572179438023,0.466318451322664,93.0322789585416));
#12971=CARTESIAN_POINT('Ctrl Pts',(2.42111811995924,0.386889306081384,93.0280487244731));
#12972=CARTESIAN_POINT('Ctrl Pts',(2.43260550988883,0.306547053535686,93.0238184904046));
#12973=CARTESIAN_POINT('Ctrl Pts',(2.44008296707689,0.225710796775996,93.0195882563361));
#12974=CARTESIAN_POINT('Ctrl Pts',(2.44754966236895,0.144990883228411,93.0153641106126));
#12975=CARTESIAN_POINT('Ctrl Pts',(2.4510178444076,0.0637788367834349,93.0111399648891));
#12976=CARTESIAN_POINT('Ctrl Pts',(2.4504375392987,-0.0174961708875144,
93.0069158191656));
#12977=CARTESIAN_POINT('Ctrl Pts',(2.44985423478089,-0.099191262715211,
93.0026698402028));
#12978=CARTESIAN_POINT('Ctrl Pts',(2.44518037701346,-0.180949501444377,
92.99842386124));
#12979=CARTESIAN_POINT('Ctrl Pts',(2.43641812250323,-0.262329911252715,
92.9941778822772));
#12980=CARTESIAN_POINT('Ctrl Pts',(2.42771670165569,-0.34314532167704,92.9899613818523));
#12981=CARTESIAN_POINT('Ctrl Pts',(2.41498352373129,-0.423587664264211,
92.9857448814274));
#12982=CARTESIAN_POINT('Ctrl Pts',(2.39827287353054,-0.503227060170226,
92.9815283810025));
#12983=CARTESIAN_POINT('Ctrl Pts',(2.38156778355595,-0.582839957223856,
92.977313283557));
#12984=CARTESIAN_POINT('Ctrl Pts',(2.36088794486213,-0.661649983233959,
92.9730981861114));
#12985=CARTESIAN_POINT('Ctrl Pts',(2.33633890883861,-0.739236601533515,
92.9688830886658));
#12986=CARTESIAN_POINT('Ctrl Pts',(2.31179051031042,-0.8168212050449,92.9646681006788));
#12987=CARTESIAN_POINT('Ctrl Pts',(2.28337325556862,-0.893182020818318,
92.9604531126919));
#12988=CARTESIAN_POINT('Ctrl Pts',(2.25124238673006,-0.967914234935082,
92.956238124705));
#12989=CARTESIAN_POINT('Ctrl Pts',(2.21870118125789,-1.04360083859284,92.9519693079844));
#12990=CARTESIAN_POINT('Ctrl Pts',(2.18235101290933,-1.11761649190415,92.9477004912638));
#12991=CARTESIAN_POINT('Ctrl Pts',(2.14240240208921,-1.1895638686184,92.9434316745432));
#12992=CARTESIAN_POINT('Ctrl Pts',(2.10290000319201,-1.26070761845669,92.939210539003));
#12993=CARTESIAN_POINT('Ctrl Pts',(2.05987944975525,-1.32982869849066,92.9349894034628));
#12994=CARTESIAN_POINT('Ctrl Pts',(2.01358840145199,-1.39657151608431,92.9307682679226));
#12995=CARTESIAN_POINT('Ctrl Pts',(1.96651301023838,-1.46444520579503,92.9264756106118));
#12996=CARTESIAN_POINT('Ctrl Pts',(1.91605557430884,-1.52985889405666,92.922182953301));
#12997=CARTESIAN_POINT('Ctrl Pts',(1.86251844080857,-1.59247458618592,92.9178902959903));
#12998=CARTESIAN_POINT('Ctrl Pts',(1.80898130730829,-1.65509027831519,92.9135976386795));
#12999=CARTESIAN_POINT('Ctrl Pts',(1.75236486738772,-1.71490765797517,92.9093049813687));
#13000=CARTESIAN_POINT('Ctrl Pts',(1.69300821898914,-1.77163015904427,92.9050123240579));
#13001=CARTESIAN_POINT('Ctrl Pts',(1.63451472488171,-1.82752781114492,92.9007820898401));
#13002=CARTESIAN_POINT('Ctrl Pts',(1.57313961198365,-1.88063085808535,92.8965518556222));
#13003=CARTESIAN_POINT('Ctrl Pts',(1.50918083421384,-1.93062773719887,92.8923216214044));
#13004=CARTESIAN_POINT('Ctrl Pts',(1.44531410883259,-1.98055265852483,92.8880974755325));
#13005=CARTESIAN_POINT('Ctrl Pts',(1.37887146708518,-2.02738000662939,92.8838733296605));
#13006=CARTESIAN_POINT('Ctrl Pts',(1.31018692013596,-2.07083569708092,92.8796491837886));
#13007=CARTESIAN_POINT('Ctrl Pts',(1.24114736806969,-2.11451599398559,92.875403204863));
#13008=CARTESIAN_POINT('Ctrl Pts',(1.16984301045906,-2.15478934675703,92.8711572259374));
#13009=CARTESIAN_POINT('Ctrl Pts',(1.09664597431824,-2.19141914224815,92.8669112470118));
#13010=CARTESIAN_POINT('Ctrl Pts',(1.02395711975321,-2.2277946298031,92.8626947464418));
#13011=CARTESIAN_POINT('Ctrl Pts',(0.949402205335669,-2.26057678084734,
92.8584782458718));
#13012=CARTESIAN_POINT('Ctrl Pts',(0.873372207824021,-2.28957883389076,
92.8542617453019));
#13013=CARTESIAN_POINT('Ctrl Pts',(0.797367508216987,-2.31857123691189,
92.8500466477127));
#13014=CARTESIAN_POINT('Ctrl Pts',(0.719889134464225,-2.34378587396247,
92.8458315501235));
#13015=CARTESIAN_POINT('Ctrl Pts',(0.641347923301296,-2.3650841615632,92.8416164525344));
#13016=CARTESIAN_POINT('Ctrl Pts',(0.562808751748022,-2.38638189607604,
92.8374014644057));
#13017=CARTESIAN_POINT('Ctrl Pts',(0.483207246910017,-2.40376336262492,
92.8331864762769));
#13018=CARTESIAN_POINT('Ctrl Pts',(0.402967885948781,-2.41714027993701,
92.8289714881482));
#13019=CARTESIAN_POINT('Ctrl Pts',(0.321703810844169,-2.4306880300698,92.8247026716004));
#13020=CARTESIAN_POINT('Ctrl Pts',(0.239785951321221,-2.44012812440312,
92.8204338550525));
#13021=CARTESIAN_POINT('Ctrl Pts',(0.157662373535208,-2.44542283173509,
92.8161650385047));
#13022=CARTESIAN_POINT('Ctrl Pts',(0.0764560813043814,-2.45065839943035,
92.8119439028283));
#13023=CARTESIAN_POINT('Ctrl Pts',(-0.00495088474896378,-2.45184077868515,
92.807722767152));
#13024=CARTESIAN_POINT('Ctrl Pts',(-0.0861254853411517,-2.44898604544304,
92.8035016314756));
#13025=CARTESIAN_POINT('Ctrl Pts',(-0.168675477295125,-2.44608294269357,
92.7992089744921));
#13026=CARTESIAN_POINT('Ctrl Pts',(-0.250984655618082,-2.43900469479108,
92.7949163175085));
#13027=CARTESIAN_POINT('Ctrl Pts',(-0.332605216569839,-2.42782289714685,
92.7906236605249));
#13028=CARTESIAN_POINT('Ctrl Pts',(-0.414225777521596,-2.41664109950263,
92.7863310035414));
#13029=CARTESIAN_POINT('Ctrl Pts',(-0.495157243503421,-2.40135591012571,
92.7820383465578));
#13030=CARTESIAN_POINT('Ctrl Pts',(-0.574966791155317,-2.38209223983215,
92.7777456895743));
#13031=CARTESIAN_POINT('Ctrl Pts',(-0.653615772711475,-2.36310869595555,
92.7735154550991));
#13032=CARTESIAN_POINT('Ctrl Pts',(-0.731471891581371,-2.34019006404083,
92.7692852206239));
#13033=CARTESIAN_POINT('Ctrl Pts',(-0.808111954547987,-2.31341853518049,
92.7650549861487));
#13034=CARTESIAN_POINT('Ctrl Pts',(-0.884641713695443,-2.28668553710631,
92.7608308400169));
#13035=CARTESIAN_POINT('Ctrl Pts',(-0.959958457488453,-2.25611080728024,
92.756606693885));
#13036=CARTESIAN_POINT('Ctrl Pts',(-1.03365102497352,-2.22182713291813,
92.7523825477532));
#13037=CARTESIAN_POINT('Ctrl Pts',(-1.10772447650297,-2.18736626151983,
92.7481365688922));
#13038=CARTESIAN_POINT('Ctrl Pts',(-1.18015644979191,-2.14915810302381,
92.7438905900313));
#13039=CARTESIAN_POINT('Ctrl Pts',(-1.25054669734552,-2.10738776872179,
92.7396446111704));
#13040=CARTESIAN_POINT('Ctrl Pts',(-1.32044825532549,-2.06590742809887,
92.7354281103362));
#13041=CARTESIAN_POINT('Ctrl Pts',(-1.38833594214196,-2.02091445690706,
92.731211609502));
#13042=CARTESIAN_POINT('Ctrl Pts',(-1.45384125510295,-1.97263677725036,
92.7269951086678));
#13043=CARTESIAN_POINT('Ctrl Pts',(-1.51932477211615,-1.92437516129503,
92.7227800108134));
#13044=CARTESIAN_POINT('Ctrl Pts',(-1.58242711524957,-1.87283128300427,
92.718564912959));
#13045=CARTESIAN_POINT('Ctrl Pts',(-1.64280957257505,-1.81827582018125,
92.7143498151046));
#13046=CARTESIAN_POINT('Ctrl Pts',(-1.70319046185879,-1.76372177408166,
92.71013482671));
#13047=CARTESIAN_POINT('Ctrl Pts',(-1.76085126131092,-1.70615661159099,
92.7059198383154));
#13048=CARTESIAN_POINT('Ctrl Pts',(-1.81548819949196,-1.64588968266571,
92.7017048499208));
#13049=CARTESIAN_POINT('Ctrl Pts',(-1.87082288299455,-1.58485311017875,
92.6974360336849));
#13050=CARTESIAN_POINT('Ctrl Pts',(-1.92305558209633,-1.5210456249169,92.6931672174491));
#13051=CARTESIAN_POINT('Ctrl Pts',(-1.97191229546202,-1.45482375187021,
92.6888984012133));
#13052=CARTESIAN_POINT('Ctrl Pts',(-2.0202233066089,-1.38934154018355,92.6846772652721));
#13053=CARTESIAN_POINT('Ctrl Pts',(-2.06523316365711,-1.32149903360087,
92.680456129331));
#13054=CARTESIAN_POINT('Ctrl Pts',(-2.10672125396135,-1.25166920873988,
92.6762349933899));
#13055=CARTESIAN_POINT('Ctrl Pts',(-2.14891229404025,-1.18065622844101,
92.6719423370067));
#13056=CARTESIAN_POINT('Ctrl Pts',(-2.18746088418393,-1.10758840587916,
92.6676496806235));
#13057=CARTESIAN_POINT('Ctrl Pts',(-2.22218513349975,-1.03288115601589,
92.6633570242403));
#13058=CARTESIAN_POINT('Ctrl Pts',(-2.25690938281556,-0.958173906152611,
92.6590643678571));
#13059=CARTESIAN_POINT('Ctrl Pts',(-2.28780916599659,-0.881827716189098,
92.6547717114739));
#13060=CARTESIAN_POINT('Ctrl Pts',(-2.31475554210733,-0.804274225798275,
92.6504790550907));
#13061=CARTESIAN_POINT('Ctrl Pts',(-2.34592638274948,-0.714562441167906,
92.6455134260391));
#13062=CARTESIAN_POINT('Ctrl Pts',(-2.37190502880027,-0.622958806512549,
92.6405477969874));
#13063=CARTESIAN_POINT('Ctrl Pts',(-2.39249357676296,-0.530023334531582,
92.6355821679358));
#13064=CARTESIAN_POINT('Ctrl Pts',(-2.41287918516334,-0.43800391957615,
92.6306654846664));
#13065=CARTESIAN_POINT('Ctrl Pts',(-2.4279803610644,-0.344678912633406,
92.6257488013971));
#13066=CARTESIAN_POINT('Ctrl Pts',(-2.43765120865071,-0.250612918589105,
92.6208321181277));
#13067=CARTESIAN_POINT('Ctrl Pts',(-2.44612937792563,-0.168147817841233,
92.6165217955157));
#13068=CARTESIAN_POINT('Ctrl Pts',(-2.45043464139583,-0.08511357872822,
92.6122114729037));
#13069=CARTESIAN_POINT('Ctrl Pts',(-2.45049926108039,-0.00190300932192698,
92.6079011502917));
#13070=CARTESIAN_POINT('',(-2.45049953842671,0.00150405135357228,91.8079011502354));
#13071=CARTESIAN_POINT('Ctrl Pts',(-2.4504992610808,-0.00190300879332999,
92.6079011502643));
#13072=CARTESIAN_POINT('Ctrl Pts',(-2.45056242607356,0.0794343810401948,
92.6036878586945));
#13073=CARTESIAN_POINT('Ctrl Pts',(-2.44657163267656,0.160818933598828,
92.5994745671246));
#13074=CARTESIAN_POINT('Ctrl Pts',(-2.43853945979514,0.241817189260865,
92.5952612755548));
#13075=CARTESIAN_POINT('Ctrl Pts',(-2.43050856615323,0.32280254478121,92.5910486550125));
#13076=CARTESIAN_POINT('Ctrl Pts',(-2.41843761755519,0.403401262967549,
92.5868360344702));
#13077=CARTESIAN_POINT('Ctrl Pts',(-2.40239111851131,0.483184399270065,
92.5826234139278));
#13078=CARTESIAN_POINT('Ctrl Pts',(-2.38634225763883,0.562979278576021,
92.5784101733445));
#13079=CARTESIAN_POINT('Ctrl Pts',(-2.36631677735233,0.641957882004794,
92.5741969327612));
#13080=CARTESIAN_POINT('Ctrl Pts',(-2.34243012355466,0.719702276127901,
92.5699836921778));
#13081=CARTESIAN_POINT('Ctrl Pts',(-2.3185158530207,0.797536555023019,92.5657655804244));
#13082=CARTESIAN_POINT('Ctrl Pts',(-2.29073163376794,0.874133330505025,
92.5615474686709));
#13083=CARTESIAN_POINT('Ctrl Pts',(-2.25924240106489,0.949091156438903,
92.5573293569174));
#13084=CARTESIAN_POINT('Ctrl Pts',(-2.22773386475762,1.02409493319728,92.5531086593671));
#13085=CARTESIAN_POINT('Ctrl Pts',(-2.19251599537294,1.09745734135112,92.5488879618168));
#13086=CARTESIAN_POINT('Ctrl Pts',(-2.15380026986483,1.16880051656824,92.5446672642665));
#13087=CARTESIAN_POINT('Ctrl Pts',(-2.11501406719797,1.24027356315465,92.5404388834616));
#13088=CARTESIAN_POINT('Ctrl Pts',(-2.0727175352075,1.30971963942041,92.5362105026568));
#13089=CARTESIAN_POINT('Ctrl Pts',(-2.02716597175543,1.37678915341342,92.531982121852));
#13090=CARTESIAN_POINT('Ctrl Pts',(-1.99567451587214,1.42315675270005,92.5290588881037));
#13091=CARTESIAN_POINT('Ctrl Pts',(-1.96262822674959,1.46838911902986,92.5261356543553));
#13092=CARTESIAN_POINT('Ctrl Pts',(-1.92812221977048,1.51238055912768,92.523212420607));
#13093=CARTESIAN_POINT('Ctrl Pts',(-1.87818830234013,1.57604092234551,92.5189821857755));
#13094=CARTESIAN_POINT('Ctrl Pts',(-1.82500404415984,1.63734568847151,92.514751950944));
#13095=CARTESIAN_POINT('Ctrl Pts',(-1.76881997612733,1.69594402680422,92.5105217161125));
#13096=CARTESIAN_POINT('Ctrl Pts',(-1.71271677083371,1.75445802766728,92.5062975696329));
#13097=CARTESIAN_POINT('Ctrl Pts',(-1.65362264953648,1.81027300386652,92.5020734231532));
#13098=CARTESIAN_POINT('Ctrl Pts',(-1.59182917166381,1.86307008409241,92.4978492766736));
#13099=CARTESIAN_POINT('Ctrl Pts',(-1.5297163172406,1.91614004343017,92.4936032979007));
#13100=CARTESIAN_POINT('Ctrl Pts',(-1.46487641363222,1.96616044360353,92.4893573191277));
#13101=CARTESIAN_POINT('Ctrl Pts',(-1.39764408523588,2.0128440727004,92.4851113403548));
#13102=CARTESIAN_POINT('Ctrl Pts',(-1.33087851579443,2.0592036017334,92.4808948391957));
#13103=CARTESIAN_POINT('Ctrl Pts',(-1.26175402222121,2.10227227508018,92.4766783380367));
#13104=CARTESIAN_POINT('Ctrl Pts',(-1.19063098829858,2.14180953861522,92.4724618368776));
#13105=CARTESIAN_POINT('Ctrl Pts',(-1.11953161969357,2.18133364661052,92.4682467387076));
#13106=CARTESIAN_POINT('Ctrl Pts',(-1.04643543753931,2.21732845233955,92.4640316405376));
#13107=CARTESIAN_POINT('Ctrl Pts',(-0.971729346338488,2.24959825912641,
92.4598165423676));
#13108=CARTESIAN_POINT('Ctrl Pts',(-0.89702519531303,2.28186722784126,92.455601553667));
#13109=CARTESIAN_POINT('Ctrl Pts',(-0.820711645839797,2.31041120646844,
92.4513865649663));
#13110=CARTESIAN_POINT('Ctrl Pts',(-0.743196269632219,2.33508234433066,
92.4471715762657));
#13111=CARTESIAN_POINT('Ctrl Pts',(-0.664690990092166,2.36006854280124,
92.4429027604205));
#13112=CARTESIAN_POINT('Ctrl Pts',(-0.584953430463237,2.38108211698799,
92.4386339445753));
#13113=CARTESIAN_POINT('Ctrl Pts',(-0.504421711694072,2.39802189038625,
92.4343651287302));
#13114=CARTESIAN_POINT('Ctrl Pts',(-0.424789474714928,2.41477245861253,
92.4301439925096));
#13115=CARTESIAN_POINT('Ctrl Pts',(-0.344381205452798,2.42753976328988,
92.4259228562889));
#13116=CARTESIAN_POINT('Ctrl Pts',(-0.263627816841055,2.43627802686549,
92.4217017200683));
#13117=CARTESIAN_POINT('Ctrl Pts',(-0.181506209679372,2.44516434434354,
92.4174090644109));
#13118=CARTESIAN_POINT('Ctrl Pts',(-0.0990281817692588,2.44988379597553,
92.4131164087534));
#13119=CARTESIAN_POINT('Ctrl Pts',(-0.0166471684788547,2.45044345410818,
92.4088237530959));
#13120=CARTESIAN_POINT('Ctrl Pts',(0.0657338448115509,2.45100311224084,
92.4045310974384));
#13121=CARTESIAN_POINT('Ctrl Pts',(0.148017348246232,2.44740306523394,92.400238441781));
#13122=CARTESIAN_POINT('Ctrl Pts',(0.229757138867459,2.43970529104223,92.3959457861235));
#13123=CARTESIAN_POINT('Ctrl Pts',(0.310308354856322,2.43211944984008,92.3917155497795));
#13124=CARTESIAN_POINT('Ctrl Pts',(0.390635373853221,2.42052570211332,92.3874853134356));
#13125=CARTESIAN_POINT('Ctrl Pts',(0.470307609770855,2.40494511417446,92.3832550770917));
#13126=CARTESIAN_POINT('Ctrl Pts',(0.54986517813793,2.38938695045698,92.3790309290774));
#13127=CARTESIAN_POINT('Ctrl Pts',(0.628769382404817,2.36985343097383,92.3748067810632));
#13128=CARTESIAN_POINT('Ctrl Pts',(0.706594338299834,2.34641741620766,92.370582633049));
#13129=CARTESIAN_POINT('Ctrl Pts',(0.784821493214441,2.32286028422331,92.3663366546569));
#13130=CARTESIAN_POINT('Ctrl Pts',(0.861957737646102,2.29536024502775,92.3620906762649));
#13131=CARTESIAN_POINT('Ctrl Pts',(0.937580536278816,2.26404350399703,92.3578446978728));
#13132=CARTESIAN_POINT('Ctrl Pts',(1.01267836012187,2.23294416432982,92.353628195137));
#13133=CARTESIAN_POINT('Ctrl Pts',(1.08628324891366,2.19808112658015,92.3494116924011));
#13134=CARTESIAN_POINT('Ctrl Pts',(1.15799798899147,2.15962749276159,92.3451951896653));
#13135=CARTESIAN_POINT('Ctrl Pts',(1.22968886708583,2.12118665380184,92.3409800899063));
#13136=CARTESIAN_POINT('Ctrl Pts',(1.29949043573397,2.07915781089497,92.3367649901472));
#13137=CARTESIAN_POINT('Ctrl Pts',(1.3670288773691,2.0337606295823,92.3325498903882));
#13138=CARTESIAN_POINT('Ctrl Pts',(1.43456556513953,1.9883646271614,92.3283349000886));
#13139=CARTESIAN_POINT('Ctrl Pts',(1.49983885726426,1.93960072063591,92.3241199097889));
#13140=CARTESIAN_POINT('Ctrl Pts',(1.56250401119836,1.88773183079299,92.3199049194892));
#13141=CARTESIAN_POINT('Ctrl Pts',(1.62596937330396,1.83520059661843,92.3156361055018));
#13142=CARTESIAN_POINT('Ctrl Pts',(1.68675912641859,1.77948481501085,92.3113672915143));
#13143=CARTESIAN_POINT('Ctrl Pts',(1.74455127498463,1.72089834067835,92.3070984775269));
#13144=CARTESIAN_POINT('Ctrl Pts',(1.80169797314627,1.66296618816099,92.3028773396993));
#13145=CARTESIAN_POINT('Ctrl Pts',(1.85591342349688,1.60222753885427,92.2986562018717));
#13146=CARTESIAN_POINT('Ctrl Pts',(1.90692613005042,1.53902013779253,92.2944350640442));
#13147=CARTESIAN_POINT('Ctrl Pts',(1.95880309052766,1.47474188109374,92.2901424119768));
#13148=CARTESIAN_POINT('Ctrl Pts',(2.00736748366151,1.40791085252572,92.2858497599094));
#13149=CARTESIAN_POINT('Ctrl Pts',(2.05238009564119,1.33891231714996,92.281557107842));
#13150=CARTESIAN_POINT('Ctrl Pts',(2.09739270762087,1.26991378177419,92.2772644557746));
#13151=CARTESIAN_POINT('Ctrl Pts',(2.13885334501351,1.19874820396808,92.2729718037073));
#13152=CARTESIAN_POINT('Ctrl Pts',(2.17657289230003,1.12582445101564,92.2686791516399));
#13153=CARTESIAN_POINT('Ctrl Pts',(2.21374390716426,1.0539611838253,92.2644489249992));
#13154=CARTESIAN_POINT('Ctrl Pts',(2.24742215915486,0.980119523096709,92.2602186983586));
#13155=CARTESIAN_POINT('Ctrl Pts',(2.27739255994902,0.904673077906526,92.255988471718));
#13156=CARTESIAN_POINT('Ctrl Pts',(2.30731982586546,0.829335218958139,92.251764333428));
#13157=CARTESIAN_POINT('Ctrl Pts',(2.33354966884192,0.752397591305803,92.247540195138));
#13158=CARTESIAN_POINT('Ctrl Pts',(2.35591311335638,0.674257852987607,92.243316056848));
#13159=CARTESIAN_POINT('Ctrl Pts',(2.37839219665573,0.595714063120693,92.2390700760275));
#13160=CARTESIAN_POINT('Ctrl Pts',(2.39696455807962,0.515956116139998,92.234824095207));
#13161=CARTESIAN_POINT('Ctrl Pts',(2.41150790699371,0.435407699181804,92.2305781143866));
#13162=CARTESIAN_POINT('Ctrl Pts',(2.42595025422533,0.355418680590661,92.2263616213552));
#13163=CARTESIAN_POINT('Ctrl Pts',(2.43641928988118,0.274650600485336,92.2221451283239));
#13164=CARTESIAN_POINT('Ctrl Pts',(2.44284586612902,0.193531197320604,92.2179286352926));
#13165=CARTESIAN_POINT('Ctrl Pts',(2.44927030407069,0.112438784907014,92.2137135452094));
#13166=CARTESIAN_POINT('Ctrl Pts',(2.45165491688449,0.0309957449287714,
92.2094984551262));
#13167=CARTESIAN_POINT('Ctrl Pts',(2.44998237708902,-0.0503646895478568,
92.205283365043));
#13168=CARTESIAN_POINT('Ctrl Pts',(2.44830988071032,-0.131723012022023,
92.2010683843776));
#13169=CARTESIAN_POINT('Ctrl Pts',(2.44258045174376,-0.212998268190724,
92.1968534037122));
#13170=CARTESIAN_POINT('Ctrl Pts',(2.43282887053207,-0.293758296403091,
92.1926384230469));
#13171=CARTESIAN_POINT('Ctrl Pts',(2.42295271646221,-0.375550004229518,
92.188369597556));
#13172=CARTESIAN_POINT('Ctrl Pts',(2.40895095771543,-0.456812739436458,
92.1841007720651));
#13173=CARTESIAN_POINT('Ctrl Pts',(2.39091352198649,-0.537105930317421,
92.1798319465742));
#13174=CARTESIAN_POINT('Ctrl Pts',(2.37307762490926,-0.616501976966011,
92.175610818181));
#13175=CARTESIAN_POINT('Ctrl Pts',(2.35129597153643,-0.694949600364978,
92.1713896897878));
#13176=CARTESIAN_POINT('Ctrl Pts',(2.3257058896982,-0.772037799996274,92.1671685613946));
#13177=CARTESIAN_POINT('Ctrl Pts',(2.29968207100601,-0.850432599324957,
92.1628758873549));
#13178=CARTESIAN_POINT('Ctrl Pts',(2.26971970688244,-0.927420995837426,
92.1585832133151));
#13179=CARTESIAN_POINT('Ctrl Pts',(2.23601355909546,-1.00259344379527,92.1542905392754));
#13180=CARTESIAN_POINT('Ctrl Pts',(2.20230741130847,-1.07776589175312,92.1499978652357));
#13181=CARTESIAN_POINT('Ctrl Pts',(2.16485776593381,-1.1511219773395,92.145705191196));
#13182=CARTESIAN_POINT('Ctrl Pts',(2.12390632801813,-1.2222815386827,92.1414125171563));
#13183=CARTESIAN_POINT('Ctrl Pts',(2.08355048458691,-1.29240616097591,92.1371822754293));
#13184=CARTESIAN_POINT('Ctrl Pts',(2.03964187030215,-1.3606622373627,92.1329520337024));
#13185=CARTESIAN_POINT('Ctrl Pts',(1.99237848348988,-1.42666682463936,92.1287217919755));
#13186=CARTESIAN_POINT('Ctrl Pts',(1.94518312073995,-1.49257641448858,92.1244976386448));
#13187=CARTESIAN_POINT('Ctrl Pts',(1.89464284330798,-1.55624057592302,92.1202734853141));
#13188=CARTESIAN_POINT('Ctrl Pts',(1.8410008124124,-1.61730215442164,92.1160493319835));
#13189=CARTESIAN_POINT('Ctrl Pts',(1.7870816445896,-1.67867920230041,92.1118033549288));
#13190=CARTESIAN_POINT('Ctrl Pts',(1.73002881512644,-1.73742628257337,92.1075573778742));
#13191=CARTESIAN_POINT('Ctrl Pts',(1.67013261929227,-1.79321144430208,92.1033114008196));
#13192=CARTESIAN_POINT('Ctrl Pts',(1.61065213296009,-1.8486094291579,92.0990948929655));
#13193=CARTESIAN_POINT('Ctrl Pts',(1.54836796895763,-1.90108615847223,92.0948783851115));
#13194=CARTESIAN_POINT('Ctrl Pts',(1.48360256763824,-1.95035219160469,92.0906618772574));
#13195=CARTESIAN_POINT('Ctrl Pts',(1.41885871729723,-1.9996018312432,92.0864467724652));
#13196=CARTESIAN_POINT('Ctrl Pts',(1.35163563914798,-2.04564261487001,92.0822316676731));
#13197=CARTESIAN_POINT('Ctrl Pts',(1.28228841405349,-2.0882257237148,92.078016562881));
#13198=CARTESIAN_POINT('Ctrl Pts',(1.2129429912952,-2.13080772582346,92.0738015676395));
#13199=CARTESIAN_POINT('Ctrl Pts',(1.14147392832452,-2.16993198930972,92.0695865723981));
#13200=CARTESIAN_POINT('Ctrl Pts',(1.06826357846448,-2.2053941092073,92.0653715771566));
#13201=CARTESIAN_POINT('Ctrl Pts',(0.994118555750534,-2.24130897220573,
92.0611027692829));
#13202=CARTESIAN_POINT('Ctrl Pts',(0.918187900633963,-2.27346728952869,
92.0568339614093));
#13203=CARTESIAN_POINT('Ctrl Pts',(0.840890848952885,-2.30170650391124,
92.0525651535356));
#13204=CARTESIAN_POINT('Ctrl Pts',(0.7644568937653,-2.32963040009752,92.0483440110389));
#13205=CARTESIAN_POINT('Ctrl Pts',(0.686687372585542,-2.35372219881254,
92.0441228685422));
#13206=CARTESIAN_POINT('Ctrl Pts',(0.608002283014224,-2.37387520182707,
92.0399017260455));
#13207=CARTESIAN_POINT('Ctrl Pts',(0.527984418799767,-2.39436955809603,
92.0356090854833));
#13208=CARTESIAN_POINT('Ctrl Pts',(0.447020175299165,-2.41079034997452,
92.0313164449212));
#13209=CARTESIAN_POINT('Ctrl Pts',(0.365559365136432,-2.42307998228722,
92.027023804359));
#13210=CARTESIAN_POINT('Ctrl Pts',(0.284098554973698,-2.43536961459993,
92.0227311637969));
#13211=CARTESIAN_POINT('Ctrl Pts',(0.202141680907314,-2.4435281042525,92.0184385232347));
#13212=CARTESIAN_POINT('Ctrl Pts',(0.120139218826632,-2.44755323090219,
92.0141458826726));
#13213=CARTESIAN_POINT('Ctrl Pts',(0.039328630761398,-2.45151985389551,
92.0099156339779));
#13214=CARTESIAN_POINT('Ctrl Pts',(-0.0418309954404525,-2.45148748266241,
92.0056853852831));
#13215=CARTESIAN_POINT('Ctrl Pts',(-0.122910461706396,-2.44741563049743,
92.0014551365884));
#13216=CARTESIAN_POINT('Ctrl Pts',(-0.203873237726811,-2.44334963857611,
91.997230976103));
#13217=CARTESIAN_POINT('Ctrl Pts',(-0.284755622299825,-2.43525573499196,
91.9930068156175));
#13218=CARTESIAN_POINT('Ctrl Pts',(-0.365125693053675,-2.42314536878663,
91.9887826551321));
#13219=CARTESIAN_POINT('Ctrl Pts',(-0.44591081842863,-2.41097246109775,
91.9845366798428));
#13220=CARTESIAN_POINT('Ctrl Pts',(-0.526177847492383,-2.3947414593674,
91.9802907045535));
#13221=CARTESIAN_POINT('Ctrl Pts',(-0.605490578364516,-2.37451708974937,
91.9760447292642));
#13222=CARTESIAN_POINT('Ctrl Pts',(-0.684253013112445,-2.35443304302896,
91.9718282138576));
#13223=CARTESIAN_POINT('Ctrl Pts',(-0.76207389349487,-2.33041098391699,
91.9676116984509));
#13224=CARTESIAN_POINT('Ctrl Pts',(-0.838535395610174,-2.30256566471163,
91.9633951830443));
#13225=CARTESIAN_POINT('Ctrl Pts',(-0.914971457248737,-2.2747296102758,
91.959180070568));
#13226=CARTESIAN_POINT('Ctrl Pts',(-0.990048602041579,-2.2430729809124,
91.9549649580918));
#13227=CARTESIAN_POINT('Ctrl Pts',(-1.06336553039165,-2.20775995044183,
91.9507498456155));
#13228=CARTESIAN_POINT('Ctrl Pts',(-1.1366805553295,-2.17244783674798,91.9465348425695));
#13229=CARTESIAN_POINT('Ctrl Pts',(-1.20823503604193,-2.13347971349964,
91.9423198395236));
#13230=CARTESIAN_POINT('Ctrl Pts',(-1.27765028948547,-2.09106671050392,
91.9381048364776));
#13231=CARTESIAN_POINT('Ctrl Pts',(-1.34795148806702,-2.04811239141515,
91.9338360374536));
#13232=CARTESIAN_POINT('Ctrl Pts',(-1.41605803946471,-2.00162487400772,
91.9295672384295));
#13233=CARTESIAN_POINT('Ctrl Pts',(-1.48160652672157,-1.95186893770459,
91.9252984394055));
#13234=CARTESIAN_POINT('Ctrl Pts',(-1.54642335906288,-1.90266837921256,
91.921077288892));
#13235=CARTESIAN_POINT('Ctrl Pts',(-1.60873862907606,-1.850272353781,91.9168561383785));
#13236=CARTESIAN_POINT('Ctrl Pts',(-1.66823549380769,-1.79497648653129,
91.9126349878651));
#13237=CARTESIAN_POINT('Ctrl Pts',(-1.72873976291179,-1.7387443464427,91.9083423645857));
#13238=CARTESIAN_POINT('Ctrl Pts',(-1.78632894863795,-1.6795136139708,91.9040497413064));
#13239=CARTESIAN_POINT('Ctrl Pts',(-1.84071139952382,-1.61763153828771,
91.899757118027));
#13240=CARTESIAN_POINT('Ctrl Pts',(-1.8950938504097,-1.55574946260462,91.8954644947477));
#13241=CARTESIAN_POINT('Ctrl Pts',(-1.94626930885375,-1.49121647577073,
91.8911718714683));
#13242=CARTESIAN_POINT('Ctrl Pts',(-1.99399234651966,-1.42441032431705,
91.886879248189));
#13243=CARTESIAN_POINT('Ctrl Pts',(-2.04145829217768,-1.35796406880582,
91.8826097499912));
#13244=CARTESIAN_POINT('Ctrl Pts',(-2.08568702951202,-1.28902010786886,
91.8783402517934));
#13245=CARTESIAN_POINT('Ctrl Pts',(-2.12640843309736,-1.21792340713709,
91.8740707535956));
#13246=CARTESIAN_POINT('Ctrl Pts',(-2.16706882103362,-1.14693323542842,
91.8698076526773));
#13247=CARTESIAN_POINT('Ctrl Pts',(-2.20423209025483,-1.07379712098361,
91.8655445517591));
#13248=CARTESIAN_POINT('Ctrl Pts',(-2.23767023184873,-0.998890476227515,
91.8612814508409));
#13249=CARTESIAN_POINT('Ctrl Pts',(-2.2725614624977,-0.920728685687057,
91.8568330924595));
#13250=CARTESIAN_POINT('Ctrl Pts',(-2.30339612314618,-0.840639372995289,
91.8523847340781));
#13251=CARTESIAN_POINT('Ctrl Pts',(-2.32996742028762,-0.759079752330567,
91.8479363756967));
#13252=CARTESIAN_POINT('Ctrl Pts',(-2.35537480837413,-0.681092707761914,
91.8436828698501));
#13253=CARTESIAN_POINT('Ctrl Pts',(-2.37688432399493,-0.601761941124336,
91.8394293640035));
#13254=CARTESIAN_POINT('Ctrl Pts',(-2.39436418876273,-0.521507796270208,
91.8351758581569));
#13255=CARTESIAN_POINT('Ctrl Pts',(-2.41183415697063,-0.441299088835756,
91.830924760514));
#13256=CARTESIAN_POINT('Ctrl Pts',(-2.42527891340726,-0.360168485131073,
91.826673662871));
#13257=CARTESIAN_POINT('Ctrl Pts',(-2.43461712473377,-0.278549288193404,
91.8224225652281));
#13258=CARTESIAN_POINT('Ctrl Pts',(-2.44395324096001,-0.196948403156809,
91.818172421352));
#13259=CARTESIAN_POINT('Ctrl Pts',(-2.44918459184153,-0.11485959340377,
91.8139222774759));
#13260=CARTESIAN_POINT('Ctrl Pts',(-2.45028150676759,-0.032722890959208,
91.8096721335998));
#13261=CARTESIAN_POINT('Ctrl Pts',(-2.45043386381017,-0.0213144355044843,
91.8090818058213));
#13262=CARTESIAN_POINT('Ctrl Pts',(-2.45050654103334,-0.0099050608674649,
91.8084914780428));
#13263=CARTESIAN_POINT('Ctrl Pts',(-2.45049953842705,0.00150405079498821,
91.8079011502643));
#13264=CARTESIAN_POINT('Ctrl Pts',(-2.45049953842671,0.00150405135356907,
91.8079011502354));
#13265=CARTESIAN_POINT('Ctrl Pts',(-2.45044342734625,0.0929239197229016,
91.8031709232553));
#13266=CARTESIAN_POINT('Ctrl Pts',(-2.44526737934698,0.184152685350111,
91.7984406962751));
#13267=CARTESIAN_POINT('Ctrl Pts',(-2.43505973922788,0.274653083710055,
91.793710469295));
#13268=CARTESIAN_POINT('Ctrl Pts',(-2.42480793863696,0.365545006481651,
91.7889597783239));
#13269=CARTESIAN_POINT('Ctrl Pts',(-2.40948104789849,0.455702014559125,
91.7842090873527));
#13270=CARTESIAN_POINT('Ctrl Pts',(-2.38921823372468,0.544597540976377,
91.7794583963816));
#13271=CARTESIAN_POINT('Ctrl Pts',(-2.3688459255397,0.633973431457541,91.7746820341387));
#13272=CARTESIAN_POINT('Ctrl Pts',(-2.34348433095867,0.722073944947803,
91.7699056718958));
#13273=CARTESIAN_POINT('Ctrl Pts',(-2.31332305585638,0.808385235666317,
91.7651293096528));
#13274=CARTESIAN_POINT('Ctrl Pts',(-2.30171097008438,0.841615067877205,
91.7632904110037));
#13275=CARTESIAN_POINT('Ctrl Pts',(-2.28938794702891,0.874579933837566,
91.7614515123545));
#13276=CARTESIAN_POINT('Ctrl Pts',(-2.27636663418872,0.907251451777459,
91.7596126137053));
#13277=CARTESIAN_POINT('Ctrl Pts',(-2.24641162225297,0.982410978459588,
91.7553823005517));
#13278=CARTESIAN_POINT('Ctrl Pts',(-2.21267377992271,1.05622707003952,91.7511519873981));
#13279=CARTESIAN_POINT('Ctrl Pts',(-2.17529454185354,1.12829247368853,91.7469216742446));
#13280=CARTESIAN_POINT('Ctrl Pts',(-2.13796910395373,1.20025415315478,91.742697449807));
#13281=CARTESIAN_POINT('Ctrl Pts',(-2.09701289166299,1.27046973965804,91.7384732253694));
#13282=CARTESIAN_POINT('Ctrl Pts',(-2.05261571545128,1.33855107287037,91.7342490009318));
#13283=CARTESIAN_POINT('Ctrl Pts',(-2.00799010351738,1.40698270332787,91.7300030416939));
#13284=CARTESIAN_POINT('Ctrl Pts',(-1.95988818922199,1.47325761065391,91.7257570824559));
#13285=CARTESIAN_POINT('Ctrl Pts',(-1.90855001117378,1.53700588965968,91.721511123218));
#13286=CARTESIAN_POINT('Ctrl Pts',(-1.85756708751065,1.6003130377855,91.7172945455378));
#13287=CARTESIAN_POINT('Ctrl Pts',(-1.80339284340111,1.66112804808693,91.7130779678575));
#13288=CARTESIAN_POINT('Ctrl Pts',(-1.74630520492977,1.71911848958563,91.7088613901772));
#13289=CARTESIAN_POINT('Ctrl Pts',(-1.68923657085335,1.77708962614755,91.7046462161897));
#13290=CARTESIAN_POINT('Ctrl Pts',(-1.62925679445037,1.83223772992246,91.7004310422023));
#13291=CARTESIAN_POINT('Ctrl Pts',(-1.56668189637093,1.88426592751224,91.6962158682148));
#13292=CARTESIAN_POINT('Ctrl Pts',(-1.50410863527495,1.93629276402433,91.6920008044979));
#13293=CARTESIAN_POINT('Ctrl Pts',(-1.43894074584348,1.98519956004807,91.687785740781));
#13294=CARTESIAN_POINT('Ctrl Pts',(-1.37152757036941,2.03072951761592,91.6835706770642));
#13295=CARTESIAN_POINT('Ctrl Pts',(-1.30325617171834,2.0768391076452,91.6793019522439));
#13296=CARTESIAN_POINT('Ctrl Pts',(-1.23268230853496,2.11948498222502,91.6750332274237));
#13297=CARTESIAN_POINT('Ctrl Pts',(-1.16019774959019,2.15844653207946,91.6707645026035));
#13298=CARTESIAN_POINT('Ctrl Pts',(-1.08852003537,2.19697439065649,91.6665432940841));
#13299=CARTESIAN_POINT('Ctrl Pts',(-1.01497440321775,2.23189939398055,91.6623220855646));
#13300=CARTESIAN_POINT('Ctrl Pts',(-0.939961375172089,2.26305608927057,
91.6581008770451));
#13301=CARTESIAN_POINT('Ctrl Pts',(-0.863681763782927,2.29473886052793,
91.6538083940745));
#13302=CARTESIAN_POINT('Ctrl Pts',(-0.785885218093811,2.32252472344326,
91.649515911104));
#13303=CARTESIAN_POINT('Ctrl Pts',(-0.707008699244591,2.34629259667086,
91.6452234281334));
#13304=CARTESIAN_POINT('Ctrl Pts',(-0.628132180395372,2.37006046989846,
91.6409309451628));
#13305=CARTESIAN_POINT('Ctrl Pts',(-0.548176188274773,2.38981029854057,
91.6366384621923));
#13306=CARTESIAN_POINT('Ctrl Pts',(-0.467586229601472,2.40547570511262,
91.6323459792217));
#13307=CARTESIAN_POINT('Ctrl Pts',(-0.388163321044419,2.42091425569838,
91.6281156571311));
#13308=CARTESIAN_POINT('Ctrl Pts',(-0.307825265043799,2.43244415440366,
91.6238853350405));
#13309=CARTESIAN_POINT('Ctrl Pts',(-0.226991131958893,2.43996419564141,
91.6196550129499));
#13310=CARTESIAN_POINT('Ctrl Pts',(-0.146273314150721,2.44747341600876,
91.615430778029));
#13311=CARTESIAN_POINT('Ctrl Pts',(-0.0650612961559804,2.45098419550811,
91.6112065431081));
#13312=CARTESIAN_POINT('Ctrl Pts',(0.0162157584592155,2.45044634692898,
91.6069823081872));
#13313=CARTESIAN_POINT('Ctrl Pts',(0.0979107564963627,2.44990573262124,
91.6027363513768));
#13314=CARTESIAN_POINT('Ctrl Pts',(0.179670994974369,2.44527463812407,91.5984903945665));
#13315=CARTESIAN_POINT('Ctrl Pts',(0.261055515603077,2.43655499994833,91.5942444377561));
#13316=CARTESIAN_POINT('Ctrl Pts',(0.341877181482125,2.42789566672647,91.590027845952));
#13317=CARTESIAN_POINT('Ctrl Pts',(0.422327841458038,2.41520421422521,91.5858112541478));
#13318=CARTESIAN_POINT('Ctrl Pts',(0.501977573320803,2.39853471225308,91.5815946623437));
#13319=CARTESIAN_POINT('Ctrl Pts',(0.581600815022473,2.38187075427692,91.5773794729071));
#13320=CARTESIAN_POINT('Ctrl Pts',(0.660423202646158,2.36123146932777,91.5731642834705));
#13321=CARTESIAN_POINT('Ctrl Pts',(0.738024130354673,2.33672219851103,91.5689490940339));
#13322=CARTESIAN_POINT('Ctrl Pts',(0.815623051852268,2.31221356133062,91.5647340135722));
#13323=CARTESIAN_POINT('Ctrl Pts',(0.892000132975834,2.2838352783163,91.5605189331106));
#13324=CARTESIAN_POINT('Ctrl Pts',(0.966750465322902,2.2517423893061,91.5563038526489));
#13325=CARTESIAN_POINT('Ctrl Pts',(1.04245184725185,2.21924118199528,91.5520351436564));
#13326=CARTESIAN_POINT('Ctrl Pts',(1.11648433699277,2.18293035398683,91.5477664346638));
#13327=CARTESIAN_POINT('Ctrl Pts',(1.18845054046122,2.14302019656312,91.5434977256712));
#13328=CARTESIAN_POINT('Ctrl Pts',(1.25961626549693,2.10355395890626,91.539276497431));
#13329=CARTESIAN_POINT('Ctrl Pts',(1.3287610757537,2.06056836668343,91.5350552691908));
#13330=CARTESIAN_POINT('Ctrl Pts',(1.39552923478034,2.01431090074829,91.5308340409505));
#13331=CARTESIAN_POINT('Ctrl Pts',(1.4634239151331,1.96727297264933,91.5265415915818));
#13332=CARTESIAN_POINT('Ctrl Pts',(1.52886060679971,1.91685205044352,91.522249142213));
#13333=CARTESIAN_POINT('Ctrl Pts',(1.59150121153463,1.86335024718484,91.5179566928443));
#13334=CARTESIAN_POINT('Ctrl Pts',(1.65414181626955,1.80984844392616,91.5136642434755));
#13335=CARTESIAN_POINT('Ctrl Pts',(1.7139860176476,1.75326615043448,91.5093717941068));
#13336=CARTESIAN_POINT('Ctrl Pts',(1.77073711415668,1.69394224297881,91.505079344738));
#13337=CARTESIAN_POINT('Ctrl Pts',(1.82665877833745,1.63548537016586,91.5008496306554));
#13338=CARTESIAN_POINT('Ctrl Pts',(1.87978820444791,1.57414593479859,91.4966199165727));
#13339=CARTESIAN_POINT('Ctrl Pts',(1.9298136963886,1.51022162189229,91.49239020249));
#13340=CARTESIAN_POINT('Ctrl Pts',(1.97976716813481,1.4463893388945,91.4881665777993));
#13341=CARTESIAN_POINT('Ctrl Pts',(2.02662529621523,1.37997993239357,91.4839429531086));
#13342=CARTESIAN_POINT('Ctrl Pts',(2.0701138382201,1.31132717001122,91.479719328418));
#13343=CARTESIAN_POINT('Ctrl Pts',(2.11383389079293,1.24230893573033,91.4754732193278));
#13344=CARTESIAN_POINT('Ctrl Pts',(2.15414804167968,1.1710237309849,91.4712271102377));
#13345=CARTESIAN_POINT('Ctrl Pts',(2.19081938999678,1.09784363659591,91.4669810011475));
#13346=CARTESIAN_POINT('Ctrl Pts',(2.22723053503344,1.02518279501591,91.4627650205246));
#13347=CARTESIAN_POINT('Ctrl Pts',(2.26005019472744,0.950654289210813,91.4585490399016));
#13348=CARTESIAN_POINT('Ctrl Pts',(2.28909142064245,0.874648911244454,91.4543330592786));
#13349=CARTESIAN_POINT('Ctrl Pts',(2.31812299334254,0.798668797233951,91.4501184800347));
#13350=CARTESIAN_POINT('Ctrl Pts',(2.34337846034257,0.721213220216567,91.4459039007909));
#13351=CARTESIAN_POINT('Ctrl Pts',(2.36471904008228,0.642692859359994,91.441689321547));
#13352=CARTESIAN_POINT('Ctrl Pts',(2.38605907715239,0.564174495197691,91.4374748494757));
#13353=CARTESIAN_POINT('Ctrl Pts',(2.40348430388506,0.484591850334117,91.4332603774044));
#13354=CARTESIAN_POINT('Ctrl Pts',(2.4169062337319,0.404369271023259,91.429045905333));
#13355=CARTESIAN_POINT('Ctrl Pts',(2.43050319871624,0.323100510547673,91.4247764724098));
#13356=CARTESIAN_POINT('Ctrl Pts',(2.43999159786059,0.241175483715299,91.4205070394866));
#13357=CARTESIAN_POINT('Ctrl Pts',(2.44533346016253,0.159042505669277,91.4162376065634));
#13358=CARTESIAN_POINT('Ctrl Pts',(2.45061426143794,0.0778483619974146,
91.4120169760881));
#13359=CARTESIAN_POINT('Ctrl Pts',(2.45184289289478,-0.00354853112366331,
91.4077963456128));
#13360=CARTESIAN_POINT('Ctrl Pts',(2.44903523501604,-0.084715214984909,
91.4035757151376));
#13361=CARTESIAN_POINT('Ctrl Pts',(2.44617888041592,-0.167289674137563,
91.3992818809904));
#13362=CARTESIAN_POINT('Ctrl Pts',(2.43914493860046,-0.249625360627648,
91.3949880468432));
#13363=CARTESIAN_POINT('Ctrl Pts',(2.42800489733757,-0.331274008193782,
91.390694212696));
#13364=CARTESIAN_POINT('Ctrl Pts',(2.41686485607468,-0.412922655759917,
91.3864003785488));
#13365=CARTESIAN_POINT('Ctrl Pts',(2.40161887361233,-0.493883785700159,
91.3821065444016));
#13366=CARTESIAN_POINT('Ctrl Pts',(2.38239184086457,-0.573724120620635,
91.3778127102544));
#13367=CARTESIAN_POINT('Ctrl Pts',(2.36344610079998,-0.65239638648284,91.3735816951674));
#13368=CARTESIAN_POINT('Ctrl Pts',(2.34056358204653,-0.730277318983722,
91.3693506800805));
#13369=CARTESIAN_POINT('Ctrl Pts',(2.3138263385451,-0.806943569932234,91.3651196649935));
#13370=CARTESIAN_POINT('Ctrl Pts',(2.28712758553652,-0.883499453415827,
91.3608947408058));
#13371=CARTESIAN_POINT('Ctrl Pts',(2.25658528062193,-0.958843692905802,
91.3566698166181));
#13372=CARTESIAN_POINT('Ctrl Pts',(2.2223320783732,-1.03256495361476,91.3524448924303));
#13373=CARTESIAN_POINT('Ctrl Pts',(2.18790975680346,-1.10665020042534,91.3481991084029));
#13374=CARTESIAN_POINT('Ctrl Pts',(2.1497399014367,-1.17909593443739,91.3439533243754));
#13375=CARTESIAN_POINT('Ctrl Pts',(2.10800736336254,-1.24950198319543,91.3397075403479));
#13376=CARTESIAN_POINT('Ctrl Pts',(2.06655512274216,-1.31943514827307,91.3354902732165));
#13377=CARTESIAN_POINT('Ctrl Pts',(2.0215881497874,-1.38735553784634,91.3312730060851));
#13378=CARTESIAN_POINT('Ctrl Pts',(1.97333424201925,-1.45289442812419,91.3270557389538));
#13379=CARTESIAN_POINT('Ctrl Pts',(1.92509645660628,-1.51841142087464,91.3228398808747));
#13380=CARTESIAN_POINT('Ctrl Pts',(1.873574192722,-1.58154812028761,91.3186240227956));
#13381=CARTESIAN_POINT('Ctrl Pts',(1.81903801958421,-1.64196557007361,91.3144081647165));
#13382=CARTESIAN_POINT('Ctrl Pts',(1.76450335372716,-1.70238135003107,91.310192423156));
#13383=CARTESIAN_POINT('Ctrl Pts',(1.70695525659306,-1.76007768531773,91.3059766815956));
#13384=CARTESIAN_POINT('Ctrl Pts',(1.64670299005559,-1.81475053727557,91.3017609400351));
#13385=CARTESIAN_POINT('Ctrl Pts',(1.58570518757162,-1.87009988787445,91.2974930346798));
#13386=CARTESIAN_POINT('Ctrl Pts',(1.5219361831133,-1.92235007568659,91.2932251293244));
#13387=CARTESIAN_POINT('Ctrl Pts',(1.45575201339009,-1.97122711160097,91.288957223969));
#13388=CARTESIAN_POINT('Ctrl Pts',(1.39028182267432,-2.01957687373168,91.2847353597568));
#13389=CARTESIAN_POINT('Ctrl Pts',(1.32244875105379,-2.06462570294899,91.2805134955446));
#13390=CARTESIAN_POINT('Ctrl Pts',(1.25262573029115,-2.10615266061427,91.2762916313323));
#13391=CARTESIAN_POINT('Ctrl Pts',(1.18166053694928,-2.14835892077643,91.2720007054054));
#13392=CARTESIAN_POINT('Ctrl Pts',(1.1086401497209,-2.18692681906497,91.2677097794785));
#13393=CARTESIAN_POINT('Ctrl Pts',(1.03397925625825,-2.22167440180321,91.2634188535516));
#13394=CARTESIAN_POINT('Ctrl Pts',(0.959318362795604,-2.25642198454144,
91.2591279276247));
#13395=CARTESIAN_POINT('Ctrl Pts',(0.883017448585974,-2.28734912631146,
91.2548370016978));
#13396=CARTESIAN_POINT('Ctrl Pts',(0.805507440379614,-2.31432668685583,
91.2505460757709));
#13397=CARTESIAN_POINT('Ctrl Pts',(0.72908587596123,-2.34092541170054,91.2463154056971));
#13398=CARTESIAN_POINT('Ctrl Pts',(0.651201682846937,-2.36378481128142,
91.2420847356233));
#13399=CARTESIAN_POINT('Ctrl Pts',(0.572255344369428,-2.38274507046822,
91.2378540655495));
#13400=CARTESIAN_POINT('Ctrl Pts',(0.493422431226035,-2.40167808869902,
91.2336294738471));
#13401=CARTESIAN_POINT('Ctrl Pts',(0.413530851853179,-2.4167229848221,91.2294048821447));
#13402=CARTESIAN_POINT('Ctrl Pts',(0.332998335664766,-2.42776900846116,
91.2251802904423));
#13403=CARTESIAN_POINT('Ctrl Pts',(0.252060220197776,-2.43887066502256,
91.2209344217275));
#13404=CARTESIAN_POINT('Ctrl Pts',(0.170475142269413,-2.44593289574067,
91.2166885530127));
#13405=CARTESIAN_POINT('Ctrl Pts',(0.0886797803512509,-2.4488948827087,
91.2124426842979));
#13406=CARTESIAN_POINT('Ctrl Pts',(0.00744119817062207,-2.45183670747819,
91.2082257171445));
#13407=CARTESIAN_POINT('Ctrl Pts',(-0.0740043433872743,-2.45073391836519,
91.204008749991));
#13408=CARTESIAN_POINT('Ctrl Pts',(-0.15522353275677,-2.44557884863247,
91.1997917828375));
#13409=CARTESIAN_POINT('Ctrl Pts',(-0.236415829701173,-2.44042548579103,
91.1955762119609));
#13410=CARTESIAN_POINT('Ctrl Pts',(-0.317381459527211,-2.43122253623513,
91.1913606410842));
#13411=CARTESIAN_POINT('Ctrl Pts',(-0.397689036467322,-2.41801440861582,
91.1871450702076));
#13412=CARTESIAN_POINT('Ctrl Pts',(-0.477994642849909,-2.40480660509264,
91.1829296027711));
#13413=CARTESIAN_POINT('Ctrl Pts',(-0.557641769726736,-2.38759389544172,
91.1787141353346));
#13414=CARTESIAN_POINT('Ctrl Pts',(-0.636207495698802,-2.36647211528398,
91.1744986678981));
#13415=CARTESIAN_POINT('Ctrl Pts',(-0.715757308046921,-2.3450857712107,
91.1702303990138));
#13416=CARTESIAN_POINT('Ctrl Pts',(-0.794197964003815,-2.31969185603068,
91.1659621301296));
#13417=CARTESIAN_POINT('Ctrl Pts',(-0.871106359442046,-2.29044187015074,
91.1616938612453));
#13418=CARTESIAN_POINT('Ctrl Pts',(-0.94717428986041,-2.26151153194806,
91.1574722365626));
#13419=CARTESIAN_POINT('Ctrl Pts',(-1.02174288005474,-2.22880923791292,
91.1532506118798));
#13420=CARTESIAN_POINT('Ctrl Pts',(-1.09442471470152,-2.19252931425112,
91.1490289871971));
#13421=CARTESIAN_POINT('Ctrl Pts',(-1.16831112805704,-2.15564811210192,
91.1447373962121));
#13422=CARTESIAN_POINT('Ctrl Pts',(-1.2402472411976,-2.11506986323518,91.1404458052271));
#13423=CARTESIAN_POINT('Ctrl Pts',(-1.30985564224241,-2.07104525457213,
91.1361542142421));
#13424=CARTESIAN_POINT('Ctrl Pts',(-1.37946404328721,-2.02702064590908,
91.1318626232571));
#13425=CARTESIAN_POINT('Ctrl Pts',(-1.44674436398691,-1.97955001863733,
91.1275710322721));
#13426=CARTESIAN_POINT('Ctrl Pts',(-1.51135488719631,-1.92892629588272,
91.1232794412872));
#13427=CARTESIAN_POINT('Ctrl Pts',(-1.57421989033043,-1.87967022533033,
91.1191037920691));
#13428=CARTESIAN_POINT('Ctrl Pts',(-1.63480814000601,-1.82723268945927,
91.1149281428509));
#13429=CARTESIAN_POINT('Ctrl Pts',(-1.69277337230466,-1.77185455385489,
91.1107524936328));
#13430=CARTESIAN_POINT('Ctrl Pts',(-1.75226314360995,-1.71501992227015,
91.1064670209937));
#13431=CARTESIAN_POINT('Ctrl Pts',(-1.80898952372527,-1.65508806093937,
91.1021815483546));
#13432=CARTESIAN_POINT('Ctrl Pts',(-1.86261122648677,-1.59236605997661,
91.0978960757154));
#13433=CARTESIAN_POINT('Ctrl Pts',(-1.91472175221152,-1.53141170238721,
91.0937313770822));
#13434=CARTESIAN_POINT('Ctrl Pts',(-1.9638999286895,-1.46782276849848,91.0895666784489));
#13435=CARTESIAN_POINT('Ctrl Pts',(-2.00986862981078,-1.40191952012323,
91.0854019798157));
#13436=CARTESIAN_POINT('Ctrl Pts',(-2.05580954463358,-1.33605610770776,
91.0812397985813));
#13437=CARTESIAN_POINT('Ctrl Pts',(-2.09854455984026,-1.26788154730045,
91.077077617347));
#13438=CARTESIAN_POINT('Ctrl Pts',(-2.13783760634789,-1.19774814501411,
91.0729154361127));
#13439=CARTESIAN_POINT('Ctrl Pts',(-2.17711968999981,-1.12763431011787,
91.0687544161371));
#13440=CARTESIAN_POINT('Ctrl Pts',(-2.2129614780551,-1.05556313547689,91.0645933961615));
#13441=CARTESIAN_POINT('Ctrl Pts',(-2.24517177871854,-0.981913404555533,
91.0604323761858));
#13442=CARTESIAN_POINT('Ctrl Pts',(-2.27905863398711,-0.904430185805758,
91.0560547740282));
#13443=CARTESIAN_POINT('Ctrl Pts',(-2.30892543008363,-0.825200132907421,
91.0516771718705));
#13444=CARTESIAN_POINT('Ctrl Pts',(-2.3346068648025,-0.744688550212115,
91.0472995697128));
#13445=CARTESIAN_POINT('Ctrl Pts',(-2.35904185950792,-0.668084570784174,
91.0431344330405));
#13446=CARTESIAN_POINT('Ctrl Pts',(-2.37968821884651,-0.590321058987381,
91.0389692963682));
#13447=CARTESIAN_POINT('Ctrl Pts',(-2.3964553324695,-0.511812553068496,
91.0348041596959));
#13448=CARTESIAN_POINT('Ctrl Pts',(-2.41323215421009,-0.433258590917541,
91.0306366114197));
#13449=CARTESIAN_POINT('Ctrl Pts',(-2.42612518745693,-0.353959248289263,
91.0264690631435));
#13450=CARTESIAN_POINT('Ctrl Pts',(-2.43509548030834,-0.274336019840476,
91.0223015148672));
#13451=CARTESIAN_POINT('Ctrl Pts',(-2.44407863856889,-0.194598593847754,
91.0181279893933));
#13452=CARTESIAN_POINT('Ctrl Pts',(-2.44912781095319,-0.114536831426669,
91.0139544639194));
#13453=CARTESIAN_POINT('Ctrl Pts',(-2.45025609890484,-0.0345731077519822,
91.0097809384455));
#13454=CARTESIAN_POINT('Ctrl Pts',(-2.45042549544473,-0.0225676812227585,
91.0091543423949));
#13455=CARTESIAN_POINT('Ctrl Pts',(-2.4505066074065,-0.0105644550898491,
91.0085277463443));
#13456=CARTESIAN_POINT('Ctrl Pts',(-2.45049957974585,0.00143515344103467,
91.0079011502937));
#13457=CARTESIAN_POINT('Origin',(0.,0.,89.2710285354474));
#13458=CARTESIAN_POINT('',(-0.766343857929312,1.84166898597821,96.7230113585667));
#13459=CARTESIAN_POINT('Ctrl Pts',(-0.766343857929312,1.84166898597821,
96.7230113585667));
#13460=CARTESIAN_POINT('Ctrl Pts',(-0.689464277964599,1.87365963921433,
96.7173743733537));
#13461=CARTESIAN_POINT('Ctrl Pts',(-0.610651735565635,1.90080711524305,
96.7115687222733));
#13462=CARTESIAN_POINT('Ctrl Pts',(-0.448970235501531,1.94540048021294,
96.6998596526854));
#13463=CARTESIAN_POINT('Ctrl Pts',(-0.366223654018037,1.96266124007479,
96.6939689168249));
#13464=CARTESIAN_POINT('Ctrl Pts',(-0.234099561889875,1.9815721640297,96.6848374860735));
#13465=CARTESIAN_POINT('Ctrl Pts',(-0.185328462711493,1.9867271620772,96.6815235471886));
#13466=CARTESIAN_POINT('Ctrl Pts',(-0.0967024770106042,1.99280219464184,
96.6756112671446));
#13467=CARTESIAN_POINT('Ctrl Pts',(-0.0569165008103657,1.99433518783667,
96.6729967891622));
#13468=CARTESIAN_POINT('Ctrl Pts',(0.00799370580248113,1.99489193867091,
96.668793257551));
#13469=CARTESIAN_POINT('Ctrl Pts',(0.0330989629791975,1.99463337479979,
96.6671824926306));
#13470=CARTESIAN_POINT('Ctrl Pts',(0.0822279360528475,1.99319950556032,
96.6640576343969));
#13471=CARTESIAN_POINT('Ctrl Pts',(0.106248385720628,1.99206351897154,96.662542591882));
#13472=CARTESIAN_POINT('Ctrl Pts',(0.165381681276155,1.9881942698625,96.6588408983002));
#13473=CARTESIAN_POINT('Ctrl Pts',(0.200454519605292,1.98496492944509,96.6566698667405));
#13474=CARTESIAN_POINT('Ctrl Pts',(0.377037944035307,1.96397744647056,96.6458320796582));
#13475=CARTESIAN_POINT('Ctrl Pts',(0.516437588427071,1.93200954830316,96.6376152951654));
#13476=CARTESIAN_POINT('Ctrl Pts',(0.73321504568797,1.85713327765633,96.6242415475676));
#13477=CARTESIAN_POINT('Ctrl Pts',(0.813244187714863,1.82350742849959,96.6191518491671));
#13478=CARTESIAN_POINT('Ctrl Pts',(0.913286062133564,1.7735744696473,96.6122934593206));
#13479=CARTESIAN_POINT('Ctrl Pts',(0.935533847184037,1.76194044124667,96.6107347866518));
#13480=CARTESIAN_POINT('Ctrl Pts',(0.970385576848291,1.74286927630774,96.6082302127771));
#13481=CARTESIAN_POINT('Ctrl Pts',(0.983138112306051,1.73570760857862,96.607300141527));
#13482=CARTESIAN_POINT('Ctrl Pts',(1.0083046757042,1.72120805631167,96.6054351165978));
#13483=CARTESIAN_POINT('Ctrl Pts',(1.02072003279402,1.7138745770352,96.6045003893618));
#13484=CARTESIAN_POINT('Ctrl Pts',(1.05402456718766,1.69371210776809,96.6019553523719));
#13485=CARTESIAN_POINT('Ctrl Pts',(1.0747580272508,1.68063188882308,96.600330465321));
#13486=CARTESIAN_POINT('Ctrl Pts',(1.20926713361166,1.5922665914891,96.589546171725));
#13487=CARTESIAN_POINT('Ctrl Pts',(1.31529856772277,1.50586404027768,96.5799136498756));
#13488=CARTESIAN_POINT('Ctrl Pts',(1.47343045748685,1.34746785145387,96.5643818630868));
#13489=CARTESIAN_POINT('Ctrl Pts',(1.53105586631441,1.28161534654556,96.5583944213804));
#13490=CARTESIAN_POINT('Ctrl Pts',(1.60907128548697,1.17965878703582,96.5498377271338));
#13491=CARTESIAN_POINT('Ctrl Pts',(1.6329555797574,1.14636893495378,96.5471439367675));
#13492=CARTESIAN_POINT('Ctrl Pts',(1.66986986589846,1.09142056370508,96.5428534537705));
#13493=CARTESIAN_POINT('Ctrl Pts',(1.68354223555702,1.07021019138013,96.5412330625295));
#13494=CARTESIAN_POINT('Ctrl Pts',(1.70930821101557,1.02852233776606,96.5381148717711));
#13495=CARTESIAN_POINT('Ctrl Pts',(1.72144527078454,1.00807689089324,96.5366156556503));
#13496=CARTESIAN_POINT('Ctrl Pts',(1.75006562929069,0.957839620176097,96.5330010766669));
#13497=CARTESIAN_POINT('Ctrl Pts',(1.76615765463162,0.927832849446242,96.5308998959989));
#13498=CARTESIAN_POINT('Ctrl Pts',(1.85220642307039,0.757018273381394,96.5192293313663));
#13499=CARTESIAN_POINT('Ctrl Pts',(1.90609084977174,0.608742003608438,96.5102409505371));
#13500=CARTESIAN_POINT('Ctrl Pts',(1.96227363326658,0.369297195931189,96.4959201478483));
#13501=CARTESIAN_POINT('Ctrl Pts',(1.97675274988674,0.281679466556155,96.4907039538973));
#13502=CARTESIAN_POINT('Ctrl Pts',(1.98740272489393,0.172351968173701,96.4839186172782));
#13503=CARTESIAN_POINT('Ctrl Pts',(1.98911815303444,0.151273526339116,96.4825976539646));
#13504=CARTESIAN_POINT('Ctrl Pts',(1.99139253939414,0.116495439187971,96.4803913378564));
#13505=CARTESIAN_POINT('Ctrl Pts',(1.99214598592943,0.102809500557032,96.4795162487026));
#13506=CARTESIAN_POINT('Ctrl Pts',(1.99343313839598,0.0740272878003802,
96.4776596416079));
#13507=CARTESIAN_POINT('Ctrl Pts',(1.99393651315791,0.0589309994243547,
96.4766766780363));
#13508=CARTESIAN_POINT('Ctrl Pts',(1.99489655819254,0.0152499198006821,
96.4738087792047));
#13509=CARTESIAN_POINT('Ctrl Pts',(1.99491019654391,-0.0133397280134689,
96.4719024017577));
#13510=CARTESIAN_POINT('Ctrl Pts',(1.99140676794874,-0.18002043663416,96.4606540561745));
#13511=CARTESIAN_POINT('Ctrl Pts',(1.97416743805883,-0.31744240407428,96.4508742304591));
#13512=CARTESIAN_POINT('Ctrl Pts',(1.92798282304451,-0.515971591201918,
96.4367486009863));
#13513=CARTESIAN_POINT('Ctrl Pts',(1.90994196548938,-0.579195480206896,
96.4322449262548));
#13514=CARTESIAN_POINT('Ctrl Pts',(1.87323154609103,-0.687298229869412,
96.4245699100349));
#13515=CARTESIAN_POINT('Ctrl Pts',(1.85598376796744,-0.732598253819112,
96.4213613473285));
#13516=CARTESIAN_POINT('Ctrl Pts',(1.82681215960695,-0.801549939826431,
96.4164883691608));
#13517=CARTESIAN_POINT('Ctrl Pts',(1.81604006013559,-0.82566554055961,96.4147860418146));
#13518=CARTESIAN_POINT('Ctrl Pts',(1.79487217493784,-0.870634200771682,
96.4116134678188));
#13519=CARTESIAN_POINT('Ctrl Pts',(1.78458390273124,-0.891532616084326,
96.4101397996846));
#13520=CARTESIAN_POINT('Ctrl Pts',(1.76032033520567,-0.938714923774441,
96.4068117771997));
#13521=CARTESIAN_POINT('Ctrl Pts',(1.74611786655083,-0.96487612385816,96.4049658502308));
#13522=CARTESIAN_POINT('Ctrl Pts',(1.69773577140828,-1.04942712988325,96.3989870068363));
#13523=CARTESIAN_POINT('Ctrl Pts',(1.66116982482082,-1.10639964075085,96.3949393610025));
#13524=CARTESIAN_POINT('Ctrl Pts',(1.55070492502598,-1.26065148707727,96.3837628430489));
#13525=CARTESIAN_POINT('Ctrl Pts',(1.47067649678868,-1.35315842930146,96.376810080906));
#13526=CARTESIAN_POINT('Ctrl Pts',(1.34916027595902,-1.4700200272377,96.3669234589614));
#13527=CARTESIAN_POINT('Ctrl Pts',(1.31450841706711,-1.50108609112926,96.3641660440778));
#13528=CARTESIAN_POINT('Ctrl Pts',(1.25412309290372,-1.55152732915222,96.3594009189411));
#13529=CARTESIAN_POINT('Ctrl Pts',(1.22894836457798,-1.5715430117683,96.3574252358099));
#13530=CARTESIAN_POINT('Ctrl Pts',(1.1907449895152,-1.60043801301575,96.3544244187224));
#13531=CARTESIAN_POINT('Ctrl Pts',(1.17807593254765,-1.60978648323745,96.3534288589006));
#13532=CARTESIAN_POINT('Ctrl Pts',(1.15440921280275,-1.62682111020908,96.3515655652517));
#13533=CARTESIAN_POINT('Ctrl Pts',(1.14344248094401,-1.63454789009593,96.3507005555775));
#13534=CARTESIAN_POINT('Ctrl Pts',(1.11632363912303,-1.65324843789287,96.3485586958054));
#13535=CARTESIAN_POINT('Ctrl Pts',(1.10008703827698,-1.66409654238385,96.3472740572605));
#13536=CARTESIAN_POINT('Ctrl Pts',(1.03592154766309,-1.70561778602405,96.3421965783959));
#13537=CARTESIAN_POINT('Ctrl Pts',(0.986851562851305,-1.73447062612848,
96.3383127157537));
#13538=CARTESIAN_POINT('Ctrl Pts',(0.820819803416576,-1.82276843839361,
96.3253207793254));
#13539=CARTESIAN_POINT('Ctrl Pts',(0.699216713288035,-1.87278665220588,
96.3160649716041));
#13540=CARTESIAN_POINT('Ctrl Pts',(0.526777346696431,-1.92455748394022,
96.3037483530531));
#13541=CARTESIAN_POINT('Ctrl Pts',(0.479467565956697,-1.93688599022259,
96.3004448014942));
#13542=CARTESIAN_POINT('Ctrl Pts',(0.393081229214581,-1.9560376889607,96.2945558587287));
#13543=CARTESIAN_POINT('Ctrl Pts',(0.354164067314343,-1.96345727645721,
96.2919542562003));
#13544=CARTESIAN_POINT('Ctrl Pts',(0.290449775420704,-1.9736481732425,96.2877758430453));
#13545=CARTESIAN_POINT('Ctrl Pts',(0.265777757992345,-1.97712176171708,
96.2861773117081));
#13546=CARTESIAN_POINT('Ctrl Pts',(0.217426056269668,-1.98300772827609,
96.2830805014674));
#13547=CARTESIAN_POINT('Ctrl Pts',(0.193755595513476,-1.98546029641551,
96.2815811974058));
#13548=CARTESIAN_POINT('Ctrl Pts',(0.135517884639675,-1.99044301291466,
96.2779301255032));
#13549=CARTESIAN_POINT('Ctrl Pts',(0.100917114017489,-1.99249703752709,
96.2757935327702));
#13550=CARTESIAN_POINT('Ctrl Pts',(-0.0846046827132184,-1.99866469573425,
96.2644813767062));
#13551=CARTESIAN_POINT('Ctrl Pts',(-0.235568569189636,-1.98653714948399,
96.2558312891832));
#13552=CARTESIAN_POINT('Ctrl Pts',(-0.467079258888884,-1.94115401048026,
96.2421054116408));
#13553=CARTESIAN_POINT('Ctrl Pts',(-0.549293759465421,-1.91950917588281,
96.2371240076736));
#13554=CARTESIAN_POINT('Ctrl Pts',(-0.653413530598432,-1.88485914959843,
96.2303960326469));
#13555=CARTESIAN_POINT('Ctrl Pts',(-0.676807714353878,-1.87658584734124,
96.2288558973588));
#13556=CARTESIAN_POINT('Ctrl Pts',(-0.713541301420632,-1.86281890031191,
96.2263832292885));
#13557=CARTESIAN_POINT('Ctrl Pts',(-0.726986618235207,-1.85761294951859,
96.225466487555));
#13558=CARTESIAN_POINT('Ctrl Pts',(-0.751967370117653,-1.84762780939674,
96.2237392152045));
#13559=CARTESIAN_POINT('Ctrl Pts',(-0.763516697964149,-1.84288514972356,
96.2229309182148));
#13560=CARTESIAN_POINT('Ctrl Pts',(-0.795276188659995,-1.82949353569359,
96.2206827353197));
#13561=CARTESIAN_POINT('Ctrl Pts',(-0.815388517297554,-1.82061865370054,
96.2192303483533));
#13562=CARTESIAN_POINT('Ctrl Pts',(-0.956745625039975,-1.75543060473539,
96.2088385436923));
#13563=CARTESIAN_POINT('Ctrl Pts',(-1.07219876689463,-1.68738985317196,
96.1994087122163));
#13564=CARTESIAN_POINT('Ctrl Pts',(-1.26346208142889,-1.54706616769951,
96.1829077469186));
#13565=CARTESIAN_POINT('Ctrl Pts',(-1.34206499216761,-1.47939747836251,
96.1758034296733));
#13566=CARTESIAN_POINT('Ctrl Pts',(-1.44099180885904,-1.37982725631339,
96.1664962900924));
#13567=CARTESIAN_POINT('Ctrl Pts',(-1.46619237951386,-1.35301916270848,
96.1640873235063));
#13568=CARTESIAN_POINT('Ctrl Pts',(-1.50684058254147,-1.30730773003644,
96.1601342248655));
#13569=CARTESIAN_POINT('Ctrl Pts',(-1.52270773663096,-1.28879140229587,
96.1585726966644));
#13570=CARTESIAN_POINT('Ctrl Pts',(-1.55380657808148,-1.25112393637244,
96.1554724719422));
#13571=CARTESIAN_POINT('Ctrl Pts',(-1.5690333268361,-1.231974225023,96.1539341361716));
#13572=CARTESIAN_POINT('Ctrl Pts',(-1.60653891622527,-1.18298214739122,
96.1500886299297));
#13573=CARTESIAN_POINT('Ctrl Pts',(-1.62834201737531,-1.15278644941296,
96.1478002225663));
#13574=CARTESIAN_POINT('Ctrl Pts',(-1.71421037312574,-1.02656354170838,
96.1385323570381));
#13575=CARTESIAN_POINT('Ctrl Pts',(-1.77072946969356,-0.925672963410182,
96.1318246763964));
#13576=CARTESIAN_POINT('Ctrl Pts',(-1.86640446829326,-0.713647014422534,
96.1183375458198));
#13577=CARTESIAN_POINT('Ctrl Pts',(-1.90508938296819,-0.602814909970399,
96.1115802835439));
#13578=CARTESIAN_POINT('Ctrl Pts',(-1.9397143958746,-0.465953653239696,
96.1029131731467));
#13579=CARTESIAN_POINT('Ctrl Pts',(-1.94518526216124,-0.442559509934663,
96.1014202871065));
#13580=CARTESIAN_POINT('Ctrl Pts',(-1.95322299243668,-0.405154524452922,
96.0990069539862));
#13581=CARTESIAN_POINT('Ctrl Pts',(-1.95606475888599,-0.39120439357898,
96.0981011149668));
#13582=CARTESIAN_POINT('Ctrl Pts',(-1.96146590392185,-0.363158757678868,
96.0962662248706));
#13583=CARTESIAN_POINT('Ctrl Pts',(-1.96402323233897,-0.349063730070345,
96.0953371344684));
#13584=CARTESIAN_POINT('Ctrl Pts',(-1.97054084618067,-0.31079923640034,
96.0927984235288));
#13585=CARTESIAN_POINT('Ctrl Pts',(-1.97420803448063,-0.286583143919461,
96.0911740591993));
#13586=CARTESIAN_POINT('Ctrl Pts',(-1.99452407220678,-0.133428627739084,
96.0808146554361));
#13587=CARTESIAN_POINT('Ctrl Pts',(-1.99897871200208,-0.00319550967821111,
96.0716448358197));
#13588=CARTESIAN_POINT('Ctrl Pts',(-1.98421493596182,0.229074219302177,
96.0554570290005));
#13589=CARTESIAN_POINT('Ctrl Pts',(-1.96978438357673,0.330965986839788,
96.0484102559658));
#13590=CARTESIAN_POINT('Ctrl Pts',(-1.93963649974095,0.467099545926854,
96.039165756633));
#13591=CARTESIAN_POINT('Ctrl Pts',(-1.93072348538949,0.502671717293794,
96.0367650005118));
#13592=CARTESIAN_POINT('Ctrl Pts',(-1.914269959775,0.561418319614208,96.0328227809592));
#13593=CARTESIAN_POINT('Ctrl Pts',(-1.9072767805266,0.584735306129012,96.0312640555449));
#13594=CARTESIAN_POINT('Ctrl Pts',(-1.89240786699519,0.631203360254122,
96.0281677232443));
#13595=CARTESIAN_POINT('Ctrl Pts',(-1.88452975338433,0.654349227233851,
96.0266305062904));
#13596=CARTESIAN_POINT('Ctrl Pts',(-1.86357558941499,0.712391686724026,
96.0227847801006));
#13597=CARTESIAN_POINT('Ctrl Pts',(-1.84994329691474,0.747078285606989,
96.0204951135324));
#13598=CARTESIAN_POINT('Ctrl Pts',(-1.78872331079815,0.890877884406888,
96.0110082968231));
#13599=CARTESIAN_POINT('Ctrl Pts',(-1.73239109612273,0.99600141503258,96.0041036401483));
#13600=CARTESIAN_POINT('Ctrl Pts',(-1.66701720851842,1.09548217192407,95.9972028497351));
#13601=CARTESIAN_POINT('',(1.47651116554364,1.34124656216706,96.7230113585667));
#13602=CARTESIAN_POINT('Origin',(0.,0.,96.7230113585667));
#13603=CARTESIAN_POINT('Ctrl Pts',(1.47651116554364,1.34124656216706,96.7230113585667));
#13604=CARTESIAN_POINT('Ctrl Pts',(1.48726169713084,1.32941184037036,96.7219908152654));
#13605=CARTESIAN_POINT('Ctrl Pts',(1.49786990397611,1.31744790463115,96.7209789610056));
#13606=CARTESIAN_POINT('Ctrl Pts',(1.52331794848029,1.2880428242571,96.718536457963));
#13607=CARTESIAN_POINT('Ctrl Pts',(1.5380037652555,1.27047093129895,96.7171139473732));
#13608=CARTESIAN_POINT('Ctrl Pts',(1.60871875273944,1.18283520797476,96.7101797591838));
#13609=CARTESIAN_POINT('Ctrl Pts',(1.66028370281715,1.10929505025935,96.7048517184499));
#13610=CARTESIAN_POINT('Ctrl Pts',(1.76294204385633,0.939605223750329,96.6930911735225));
#13611=CARTESIAN_POINT('Ctrl Pts',(1.81147260227835,0.842251572081398,96.686676330969));
#13612=CARTESIAN_POINT('Ctrl Pts',(1.86702105917168,0.703511697215043,96.6775510758976));
#13613=CARTESIAN_POINT('Ctrl Pts',(1.88103569161036,0.665132139708097,96.6750297349017));
#13614=CARTESIAN_POINT('Ctrl Pts',(1.90232366891468,0.600764912572967,96.6707877605653));
#13615=CARTESIAN_POINT('Ctrl Pts',(1.91026601907129,0.575010830388535,96.6690870885901));
#13616=CARTESIAN_POINT('Ctrl Pts',(1.92433456728577,0.525878065994459,96.6658316618409));
#13617=CARTESIAN_POINT('Ctrl Pts',(1.930562447417,0.502533406960201,96.6642802941438));
#13618=CARTESIAN_POINT('Ctrl Pts',(1.94594191713059,0.44037233471568,96.6601338503895));
#13619=CARTESIAN_POINT('Ctrl Pts',(1.95435573480055,0.401386397567637,96.6575172367624));
#13620=CARTESIAN_POINT('Ctrl Pts',(1.9886706534013,0.215532385394707,96.6449523428374));
#13621=CARTESIAN_POINT('Ctrl Pts',(1.99921245983725,0.0663371280025059,
96.6345518089626));
#13622=CARTESIAN_POINT('Ctrl Pts',(1.98863755630319,-0.188790145534754,
96.6166142496946));
#13623=CARTESIAN_POINT('Ctrl Pts',(1.9757579620226,-0.294458167270419,96.6091551022331));
#13624=CARTESIAN_POINT('Ctrl Pts',(1.94975550955884,-0.421958669233819,
96.6004206196238));
#13625=CARTESIAN_POINT('Ctrl Pts',(1.94457419235579,-0.445226907383012,
96.5988381285844));
#13626=CARTESIAN_POINT('Ctrl Pts',(1.93562003260773,-0.482293486178245,
96.5963411776188));
#13627=CARTESIAN_POINT('Ctrl Pts',(1.93211387872579,-0.496153109306232,
96.5954129548742));
#13628=CARTESIAN_POINT('Ctrl Pts',(1.9248929878971,-0.523458778721541,96.5935964454786));
#13629=CARTESIAN_POINT('Ctrl Pts',(1.92118574119671,-0.536905453278055,
96.5927080254385));
#13630=CARTESIAN_POINT('Ctrl Pts',(1.91080081783194,-0.573087452185706,
96.5903315248574));
#13631=CARTESIAN_POINT('Ctrl Pts',(1.90385832913146,-0.59574539536457,96.5888582421786));
#13632=CARTESIAN_POINT('Ctrl Pts',(1.86271299958318,-0.721955597954185,
96.5807066634816));
#13633=CARTESIAN_POINT('Ctrl Pts',(1.82046326714329,-0.822702048367741,
96.5744013530623));
#13634=CARTESIAN_POINT('Ctrl Pts',(1.73035776614839,-0.996169730937496,
96.5630869894992));
#13635=CARTESIAN_POINT('Ctrl Pts',(1.68559403952925,-1.0701700091139,96.5580938729166));
#13636=CARTESIAN_POINT('Ctrl Pts',(1.61333241706799,-1.17378913762508,96.5505983245961));
#13637=CARTESIAN_POINT('Ctrl Pts',(1.58951103883648,-1.20585106812816,96.5482030087696));
#13638=CARTESIAN_POINT('Ctrl Pts',(1.54372809506867,-1.263756054616,96.5437108452052));
#13639=CARTESIAN_POINT('Ctrl Pts',(1.52203888790065,-1.28979579967673,96.5416245376087));
#13640=CARTESIAN_POINT('Ctrl Pts',(1.4844503667446,-1.33265502744519,96.5380675941928));
#13641=CARTESIAN_POINT('Ctrl Pts',(1.46890214621545,-1.34977358214357,96.5366121129104));
#13642=CARTESIAN_POINT('Ctrl Pts',(1.43687143752207,-1.38383033701437,96.5336424222148));
#13643=CARTESIAN_POINT('Ctrl Pts',(1.42037855837579,-1.40075358192053,96.5321278654982));
#13644=CARTESIAN_POINT('Ctrl Pts',(1.37756178549356,-1.44315378970357,96.5282299285628));
#13645=CARTESIAN_POINT('Ctrl Pts',(1.35083063330466,-1.46820489863795,96.5258277130424));
#13646=CARTESIAN_POINT('Ctrl Pts',(1.21956194370333,-1.5846028400713,96.5141696541504));
#13647=CARTESIAN_POINT('Ctrl Pts',(1.10638410154848,-1.66559276343198,96.504484858548));
#13648=CARTESIAN_POINT('Ctrl Pts',(0.892026206343974,-1.78743864716637,
96.4871524225396));
#13649=CARTESIAN_POINT('Ctrl Pts',(0.794138538157914,-1.8330292029446,96.479572559738));
#13650=CARTESIAN_POINT('Ctrl Pts',(0.672939327064835,-1.87793493801065,
96.4709230621138));
#13651=CARTESIAN_POINT('Ctrl Pts',(0.652720963819422,-1.88505766728064,
96.4695040321753));
#13652=CARTESIAN_POINT('Ctrl Pts',(0.619719990977928,-1.89608891691162,
96.4672309521282));
#13653=CARTESIAN_POINT('Ctrl Pts',(0.607006781943613,-1.90019705703338,
96.4663656519168));
#13654=CARTESIAN_POINT('Ctrl Pts',(0.580432425716176,-1.90849033138692,
96.464579083985));
#13655=CARTESIAN_POINT('Ctrl Pts',(0.566565708973241,-1.91265273235321,
96.4636590088358));
#13656=CARTESIAN_POINT('Ctrl Pts',(0.528322261747202,-1.92367991789518,
96.4611516998533));
#13657=CARTESIAN_POINT('Ctrl Pts',(0.503857404482164,-1.93023229019666,
96.4595812290862));
#13658=CARTESIAN_POINT('Ctrl Pts',(0.384145561165289,-1.95986310821064,
96.4520290391205));
#13659=CARTESIAN_POINT('Ctrl Pts',(0.28740181941165,-1.97636924839291,96.4463268218417));
#13660=CARTESIAN_POINT('Ctrl Pts',(0.0630431245642312,-1.99781742069559,
96.4332564475615));
#13661=CARTESIAN_POINT('Ctrl Pts',(-0.0646002763201175,-1.9977668818009,
96.4259170424308));
#13662=CARTESIAN_POINT('Ctrl Pts',(-0.231716905980416,-1.98166050821652,
96.4157668921247));
#13663=CARTESIAN_POINT('Ctrl Pts',(-0.271940152437178,-1.97654225967292,
96.4132842225398));
#13664=CARTESIAN_POINT('Ctrl Pts',(-0.336911341745153,-1.96625420323763,
96.4091938575476));
#13665=CARTESIAN_POINT('Ctrl Pts',(-0.361766956812591,-1.96183317846301,
96.4076098452906));
#13666=CARTESIAN_POINT('Ctrl Pts',(-0.410048241273102,-1.95229675879365,
96.4044922284262));
#13667=CARTESIAN_POINT('Ctrl Pts',(-0.433478843753377,-1.94722833904459,
96.40296036696));
#13668=CARTESIAN_POINT('Ctrl Pts',(-0.490610404977529,-1.9337876246722,
96.3991764045732));
#13669=CARTESIAN_POINT('Ctrl Pts',(-0.524193957378882,-1.9249554785014,
96.3969100223697));
#13670=CARTESIAN_POINT('Ctrl Pts',(-0.698209252987034,-1.8742997663812,
96.3849392493386));
#13671=CARTESIAN_POINT('Ctrl Pts',(-0.833929832856933,-1.81797789754973,
96.3747738640782));
#13672=CARTESIAN_POINT('Ctrl Pts',(-1.03617142861542,-1.70660495689043,
96.3587224166777));
#13673=CARTESIAN_POINT('Ctrl Pts',(-1.10745364032079,-1.66123458087673,
96.3528756342778));
#13674=CARTESIAN_POINT('Ctrl Pts',(-1.19572665299308,-1.59683526152002,
96.3455568179254));
#13675=CARTESIAN_POINT('Ctrl Pts',(-1.21552760319727,-1.58181473590332,
96.3439099297203));
#13676=CARTESIAN_POINT('Ctrl Pts',(-1.24649016775975,-1.55740241902504,
96.341332984309));
#13677=CARTESIAN_POINT('Ctrl Pts',(-1.25783779212775,-1.54825196703071,
96.3403881729019));
#13678=CARTESIAN_POINT('Ctrl Pts',(-1.28025092259099,-1.52976946516374,
96.338523025581));
#13679=CARTESIAN_POINT('Ctrl Pts',(-1.29131708864611,-1.52043981820306,
96.3376027058249));
#13680=CARTESIAN_POINT('Ctrl Pts',(-1.32104886500062,-1.49481481667599,
96.3351285670159));
#13681=CARTESIAN_POINT('Ctrl Pts',(-1.33951469228894,-1.47829021465366,
96.3335902885473));
#13682=CARTESIAN_POINT('Ctrl Pts',(-1.41922980598246,-1.40423460265592,
96.3269174663282));
#13683=CARTESIAN_POINT('Ctrl Pts',(-1.47712190333099,-1.34320574358376,
96.321983496009));
#13684=CARTESIAN_POINT('Ctrl Pts',(-1.58056471606123,-1.21935311586967,
96.3125878147594));
#13685=CARTESIAN_POINT('Ctrl Pts',(-1.62663977922037,-1.15717317869301,
96.3081275335765));
#13686=CARTESIAN_POINT('Ctrl Pts',(-1.69996102432062,-1.04515941785083,
96.3002865052771));
#13687=CARTESIAN_POINT('Ctrl Pts',(-1.72890541181889,-0.996549626455694,
96.2969419619351));
#13688=CARTESIAN_POINT('Ctrl Pts',(-1.77657077531404,-0.908157024875483,
96.2908914474464));
#13689=CARTESIAN_POINT('Ctrl Pts',(-1.79611587033651,-0.868861472125715,
96.2882122117647));
#13690=CARTESIAN_POINT('Ctrl Pts',(-1.82505986117596,-0.805511285070732,
96.2838886781993));
#13691=CARTESIAN_POINT('Ctrl Pts',(-1.83531542692243,-0.781862591873717,
96.2822738842904));
#13692=CARTESIAN_POINT('Ctrl Pts',(-1.85415856548235,-0.735996345457414,
96.2791368626487));
#13693=CARTESIAN_POINT('Ctrl Pts',(-1.86281211673392,-0.713810579413262,
96.2776172036745));
#13694=CARTESIAN_POINT('Ctrl Pts',(-1.8823925376729,-0.660827882326651,
96.2739802633288));
#13695=CARTESIAN_POINT('Ctrl Pts',(-1.89296360185917,-0.629907730075994,
96.2718515853403));
#13696=CARTESIAN_POINT('Ctrl Pts',(-1.93273573648114,-0.50351430244711,
96.2631197231556));
#13697=CARTESIAN_POINT('Ctrl Pts',(-1.95550613988504,-0.406183281122493,
96.256316390069));
#13698=CARTESIAN_POINT('Ctrl Pts',(-1.99167629779247,-0.174405883924532,
96.2400499008643));
#13699=CARTESIAN_POINT('Ctrl Pts',(-1.99890847523624,-0.039478339302607,
96.2305196935086));
#13700=CARTESIAN_POINT('Ctrl Pts',(-1.99108799705584,0.124285972589346,
96.2194529986591));
#13701=CARTESIAN_POINT('Ctrl Pts',(-1.98905760295722,0.153389942001873,
96.2175068260181));
#13702=CARTESIAN_POINT('Ctrl Pts',(-1.98499114611209,0.197664993924626,
96.2145876994767));
#13703=CARTESIAN_POINT('Ctrl Pts',(-1.9834178195782,0.212873411585156,96.2135924894865));
#13704=CARTESIAN_POINT('Ctrl Pts',(-1.98013094169274,0.241433553360454,
96.211739576329));
#13705=CARTESIAN_POINT('Ctrl Pts',(-1.97845688517373,0.254788282443513,
96.2108799786789));
#13706=CARTESIAN_POINT('Ctrl Pts',(-1.9738684505878,0.288614683802531,96.2087182066313));
#13707=CARTESIAN_POINT('Ctrl Pts',(-1.97077061517926,0.309060445906826,
96.2074258689083));
#13708=CARTESIAN_POINT('Ctrl Pts',(-1.9550372623991,0.403012782224272,96.2015379735637));
#13709=CARTESIAN_POINT('Ctrl Pts',(-1.9386022338701,0.475829441113306,96.1971168997327));
#13710=CARTESIAN_POINT('Ctrl Pts',(-1.89445362025812,0.63048358710917,96.1877132891303));
#13711=CARTESIAN_POINT('Ctrl Pts',(-1.86542953263183,0.711784439051225,
96.1827588419002));
#13712=CARTESIAN_POINT('Ctrl Pts',(-1.80697813392815,0.847112706339792,
96.1741611377272));
#13713=CARTESIAN_POINT('Ctrl Pts',(-1.78015194144302,0.902124304349809,
96.1705609332047));
#13714=CARTESIAN_POINT('Ctrl Pts',(-1.72869993150253,0.996373144169574,
96.1641141611748));
#13715=CARTESIAN_POINT('Ctrl Pts',(-1.70515664328039,1.03614826425857,96.1613009464872));
#13716=CARTESIAN_POINT('Ctrl Pts',(-1.67588371553814,1.08189977128651,96.1579357444606));
#13717=CARTESIAN_POINT('Ctrl Pts',(-1.67147107660237,1.08870463147012,96.1574317715579));
#13718=CARTESIAN_POINT('Ctrl Pts',(-1.66701720827332,1.09548217229703,96.1569262941178));
#13719=CARTESIAN_POINT('Ctrl Pts',(-0.873522400031092,1.789212756073,90.4848163895282));
#13720=CARTESIAN_POINT('Ctrl Pts',(-1.46965815673703,1.49816970645545,90.5272386010227));
#13721=CARTESIAN_POINT('Ctrl Pts',(-2.33738230715447,0.277481532884632,
90.6120830240118));
#13722=CARTESIAN_POINT('Ctrl Pts',(-1.49668109501954,-1.8199475688586,90.7393496584954));
#13723=CARTESIAN_POINT('Ctrl Pts',(0.721519576667083,-2.24126671624503,
90.866616292979));
#13724=CARTESIAN_POINT('Ctrl Pts',(2.27564354702501,-0.605727798775474,
90.9938829274627));
#13725=CARTESIAN_POINT('Ctrl Pts',(1.73989546947818,1.58726092695295,91.1211495619463));
#13726=CARTESIAN_POINT('Ctrl Pts',(-0.394491289803378,2.32163771660372,
91.2484161964299));
#13727=CARTESIAN_POINT('Ctrl Pts',(-2.16633358048632,0.923512996017912,
91.3756828309135));
#13728=CARTESIAN_POINT('Ctrl Pts',(-1.94817348818047,-1.32310505219048,
91.5029494653973));
#13729=CARTESIAN_POINT('Ctrl Pts',(0.0596887161652472,-2.3542100608739,
91.6302160998808));
#13730=CARTESIAN_POINT('Ctrl Pts',(2.01270081331805,-1.22267742138027,91.7574827343644));
#13731=CARTESIAN_POINT('Ctrl Pts',(2.11677850049902,1.03206715101337,91.8847493688481));
#13732=CARTESIAN_POINT('Ctrl Pts',(0.276299030076897,2.33870880557926,92.0120160033317));
#13733=CARTESIAN_POINT('Ctrl Pts',(-1.81799707544443,1.49692744562467,92.1392826378152));
#13734=CARTESIAN_POINT('Ctrl Pts',(-2.24221328773756,-0.71998981316718,
92.266549272299));
#13735=CARTESIAN_POINT('Ctrl Pts',(-0.606646986926806,-2.27549634805281,
92.3938159067825));
#13736=CARTESIAN_POINT('Ctrl Pts',(1.58620794911894,-1.74064620775171,92.5210825412663));
#13737=CARTESIAN_POINT('Ctrl Pts',(2.32191234227693,0.393227629060235,92.6483491757497));
#13738=CARTESIAN_POINT('Ctrl Pts',(0.924620103765244,2.16586758240207,92.7756158102334));
#13739=CARTESIAN_POINT('Ctrl Pts',(-1.32206313274466,1.94885963628849,92.9028824447171));
#13740=CARTESIAN_POINT('Ctrl Pts',(-2.35424914491832,-0.0584445673734767,
93.0301490792007));
#13741=CARTESIAN_POINT('Ctrl Pts',(-1.22373276785853,-2.01205936745052,
93.1574157136843));
#13742=CARTESIAN_POINT('Ctrl Pts',(1.03095084926626,-2.1173202739826,93.2846823481681));
#13743=CARTESIAN_POINT('Ctrl Pts',(2.33856399250142,-0.277530625282423,
93.4119489826516));
#13744=CARTESIAN_POINT('Ctrl Pts',(1.49788372757163,1.81720916022372,93.5392156171351));
#13745=CARTESIAN_POINT('Ctrl Pts',(-0.718809229756443,2.24259182299006,
93.6664822516189));
#13746=CARTESIAN_POINT('Ctrl Pts',(-2.2751768192432,0.607844746766972,93.7937488861024));
#13747=CARTESIAN_POINT('Ctrl Pts',(-1.74148085787701,-1.58529152456845,
93.9210155205861));
#13748=CARTESIAN_POINT('Ctrl Pts',(0.39200534075291,-2.32211898878962,94.0482821550696));
#13749=CARTESIAN_POINT('Ctrl Pts',(2.16538059562593,-0.925760055246912,
94.1755487895534));
#13750=CARTESIAN_POINT('Ctrl Pts',(1.94955526487718,1.3210371221532,94.3028154240369));
#13751=CARTESIAN_POINT('Ctrl Pts',(-0.0572053256286392,2.35427956528251,
94.4300820585206));
#13752=CARTESIAN_POINT('Ctrl Pts',(-2.01141494837865,1.22479173695497,94.5573486930042));
#13753=CARTESIAN_POINT('Ctrl Pts',(-2.11786263969355,-1.02983625776083,
94.6846153274878));
#13754=CARTESIAN_POINT('Ctrl Pts',(-0.278761581426706,-2.33841745149781,
94.8118819619715));
#13755=CARTESIAN_POINT('Ctrl Pts',(1.81642050034851,-1.49884032661424,94.939148596455));
#13756=CARTESIAN_POINT('Ctrl Pts',(2.2429697838632,0.717629216563515,95.0664152309388));
#13757=CARTESIAN_POINT('Ctrl Pts',(0.609042460650236,2.27485544869131,95.1936818654223));
#13758=CARTESIAN_POINT('Ctrl Pts',(-1.5843750171001,1.7423173159803,95.320948499906));
#13759=CARTESIAN_POINT('Ctrl Pts',(-2.32232421427614,-0.390787518315191,
95.4482151343895));
#13760=CARTESIAN_POINT('Ctrl Pts',(-0.926901358188101,-2.1648837441642,
95.5754817688732));
#13761=CARTESIAN_POINT('Ctrl Pts',(1.32001402965102,-1.95026918160178,95.7027484033568));
#13762=CARTESIAN_POINT('Ctrl Pts',(2.35430264557917,0.0560043638979313,
95.8300150378406));
#13763=CARTESIAN_POINT('Ctrl Pts',(1.22586397590062,2.01069206430939,95.957281672324));
#13764=CARTESIAN_POINT('Ctrl Pts',(-1.02874906980149,2.11856292007691,96.0845483068079));
#13765=CARTESIAN_POINT('Ctrl Pts',(-2.33821394037349,0.279669963294229,
96.2118149412912));
#13766=CARTESIAN_POINT('Ctrl Pts',(-1.49991103301835,-1.81497489952105,
96.3390815757751));
#13767=CARTESIAN_POINT('Ctrl Pts',(0.716678355738466,-2.24469053279049,
96.4663482102585));
#13768=CARTESIAN_POINT('Ctrl Pts',(2.27428213796879,-0.6072203508056,96.5936329237197));
#13769=CARTESIAN_POINT('Ctrl Pts',(1.91968396703937,0.848347233302648,96.678495425686));
#13770=CARTESIAN_POINT('Ctrl Pts',(1.47321010047682,1.33939374792847,96.7209357161579));
#13771=CARTESIAN_POINT('Ctrl Pts',(-0.941185533557266,1.92780535726628,
90.5738598409889));
#13772=CARTESIAN_POINT('Ctrl Pts',(-1.58349802631975,1.61421808356536,90.6162820524834));
#13773=CARTESIAN_POINT('Ctrl Pts',(-2.5184361772614,0.298975280509143,90.7011264754725));
#13774=CARTESIAN_POINT('Ctrl Pts',(-1.61261416413696,-1.96092089176129,
90.8283931099562));
#13775=CARTESIAN_POINT('Ctrl Pts',(0.777408556109435,-2.41487546295108,
90.9556597444397));
#13776=CARTESIAN_POINT('Ctrl Pts',(2.45191512652298,-0.652647535381667,
91.0829263789235));
#13777=CARTESIAN_POINT('Ctrl Pts',(1.87466794865983,1.71021031902061,91.210193013407));
#13778=CARTESIAN_POINT('Ctrl Pts',(-0.425048625042778,2.50147200913288,
91.3374596478906));
#13779=CARTESIAN_POINT('Ctrl Pts',(-2.33413799891161,0.995048406169388,
91.4647262823743));
#13780=CARTESIAN_POINT('Ctrl Pts',(-2.09907920377313,-1.42559290346061,
91.5919929168578));
#13781=CARTESIAN_POINT('Ctrl Pts',(0.0643122101612201,-2.53656741048728,
91.7192595513416));
#13782=CARTESIAN_POINT('Ctrl Pts',(2.16860482204746,-1.31738613820236,91.8465261858251));
#13783=CARTESIAN_POINT('Ctrl Pts',(2.28074437741244,1.11201117699887,91.9737928203088));
#13784=CARTESIAN_POINT('Ctrl Pts',(0.297701180914228,2.51986542638844,92.1010594547923));
#13785=CARTESIAN_POINT('Ctrl Pts',(-1.95881931292982,1.6128795970849,92.228326089276));
#13786=CARTESIAN_POINT('Ctrl Pts',(-2.41589535596724,-0.775760296973985,
92.3555927237596));
#13787=CARTESIAN_POINT('Ctrl Pts',(-0.653637923940244,-2.4517565255035,
92.4828593582433));
#13788=CARTESIAN_POINT('Ctrl Pts',(1.70907577741699,-1.87547683919603,92.6101259927268));
#13789=CARTESIAN_POINT('Ctrl Pts',(2.50176790733853,0.423687081010561,92.7373926272105));
#13790=CARTESIAN_POINT('Ctrl Pts',(0.996241270594892,2.3336359045686,92.8646592616943));
#13791=CARTESIAN_POINT('Ctrl Pts',(-1.42447027682906,2.09981850098307,92.9919258961778));
#13792=CARTESIAN_POINT('Ctrl Pts',(-2.53660952198573,-0.0629716894781019,
93.1191925306614));
#13793=CARTESIAN_POINT('Ctrl Pts',(-1.31852323192565,-2.16791368971812,
93.2464591651451));
#13794=CARTESIAN_POINT('Ctrl Pts',(1.11080840640544,-2.28132811672488,93.3737257996286));
#13795=CARTESIAN_POINT('Ctrl Pts',(2.51970939607493,-0.299028175609036,
93.5009924341123));
#13796=CARTESIAN_POINT('Ctrl Pts',(1.61390995272828,1.95797036571637,93.628259068596));
#13797=CARTESIAN_POINT('Ctrl Pts',(-0.774488265452751,2.41630321259872,
93.7555257030794));
#13798=CARTESIAN_POINT('Ctrl Pts',(-2.45141224595995,0.654928462378868,
93.8827923375632));
#13799=CARTESIAN_POINT('Ctrl Pts',(-1.8763761414045,-1.70808836652804,94.0100589720467));
#13800=CARTESIAN_POINT('Ctrl Pts',(0.422370114127229,-2.50199056071101,
94.1373256065305));
#13801=CARTESIAN_POINT('Ctrl Pts',(2.33311119574748,-0.997469522833716,
94.264592241014));
#13802=CARTESIAN_POINT('Ctrl Pts',(2.10056801303263,1.42336479135333,94.3918588754976));
#13803=CARTESIAN_POINT('Ctrl Pts',(-0.0616364559422705,2.53664229871441,
94.5191255099812));
#13804=CARTESIAN_POINT('Ctrl Pts',(-2.16721935387969,1.3196642288755,94.6463921444649));
#13805=CARTESIAN_POINT('Ctrl Pts',(-2.2819124941387,-1.10960747852916,94.7736587789485));
#13806=CARTESIAN_POINT('Ctrl Pts',(-0.300354481740857,-2.51955150399036,
94.9009254134322));
#13807=CARTESIAN_POINT('Ctrl Pts',(1.9571206161674,-1.61494065002954,95.0281920479158));
#13808=CARTESIAN_POINT('Ctrl Pts',(2.41671045035935,0.773216848318456,95.1554586823994));
#13809=CARTESIAN_POINT('Ctrl Pts',(0.656218951300763,2.45106598201258,95.2827253168831));
#13810=CARTESIAN_POINT('Ctrl Pts',(-1.70710086629843,1.87727739163715,95.4099919513666));
#13811=CARTESIAN_POINT('Ctrl Pts',(-2.5022116829845,-0.421057959040214,
95.5372585858503));
#13812=CARTESIAN_POINT('Ctrl Pts',(-0.998699231216256,-2.33257585812122,
95.6645252203339));
#13813=CARTESIAN_POINT('Ctrl Pts',(1.42226245000237,-2.101337229819,95.7917918548176));
#13814=CARTESIAN_POINT('Ctrl Pts',(2.53666716681318,0.0603424675943402,
95.9190584893012));
#13815=CARTESIAN_POINT('Ctrl Pts',(1.32081952355841,2.16644047513726,96.0463251237848));
#13816=CARTESIAN_POINT('Ctrl Pts',(-1.10843607688045,2.28266701831146,96.1735917582684));
#13817=CARTESIAN_POINT('Ctrl Pts',(-2.51933222887374,0.301333226959783,
96.300858392752));
#13818=CARTESIAN_POINT('Ctrl Pts',(-1.61609429346009,-1.95556303895352,
96.4281250272357));
#13819=CARTESIAN_POINT('Ctrl Pts',(0.77219233371765,-2.41856448867272,96.5553916617193));
#13820=CARTESIAN_POINT('Ctrl Pts',(2.45044826258347,-0.654255700643123,
96.6826763751803));
#13821=CARTESIAN_POINT('Ctrl Pts',(2.06838288144068,0.914060295865755,96.7675388771468));
#13822=CARTESIAN_POINT('Ctrl Pts',(1.58732510398118,1.44314332321926,96.8099791676186));
#13823=CARTESIAN_POINT('Ctrl Pts',(-1.00884866708344,2.06639795845957,90.6629032924495));
#13824=CARTESIAN_POINT('Ctrl Pts',(-1.69733789590249,1.73026646067528,90.7053255039442));
#13825=CARTESIAN_POINT('Ctrl Pts',(-2.69949004736833,0.320469028133655,
90.7901699269332));
#13826=CARTESIAN_POINT('Ctrl Pts',(-1.72854723325438,-2.10189421466399,
90.9174365614169));
#13827=CARTESIAN_POINT('Ctrl Pts',(0.83329753555179,-2.58848420965714,91.0447031959004));
#13828=CARTESIAN_POINT('Ctrl Pts',(2.62818670602095,-0.699567271987858,
91.171969830384));
#13829=CARTESIAN_POINT('Ctrl Pts',(2.00944042784148,1.83315971108825,91.2992364648678));
#13830=CARTESIAN_POINT('Ctrl Pts',(-0.455605960282178,2.68130630166204,
91.4265030993513));
#13831=CARTESIAN_POINT('Ctrl Pts',(-2.50194241733692,1.06658381632086,91.553769733835));
#13832=CARTESIAN_POINT('Ctrl Pts',(-2.24998491936581,-1.52808075473076,
91.6810363683186));
#13833=CARTESIAN_POINT('Ctrl Pts',(0.0689357041571928,-2.71892476010065,
91.8083030028023));
#13834=CARTESIAN_POINT('Ctrl Pts',(2.32450883077687,-1.41209485502446,91.9355696372858));
#13835=CARTESIAN_POINT('Ctrl Pts',(2.44471025432585,1.19195520298437,92.0628362717697));
#13836=CARTESIAN_POINT('Ctrl Pts',(0.319103331751555,2.70102204719762,92.1901029062529));
#13837=CARTESIAN_POINT('Ctrl Pts',(-2.09964155041522,1.72883174854512,92.3173695407368));
#13838=CARTESIAN_POINT('Ctrl Pts',(-2.58957742419693,-0.83153078078079,
92.4446361752204));
#13839=CARTESIAN_POINT('Ctrl Pts',(-0.700628860953678,-2.62801670295417,
92.5719028097039));
#13840=CARTESIAN_POINT('Ctrl Pts',(1.83194360571502,-2.01030747064033,92.6991694441877));
#13841=CARTESIAN_POINT('Ctrl Pts',(2.68162347240014,0.454146532960888,92.8264360786714));
#13842=CARTESIAN_POINT('Ctrl Pts',(1.06786243742454,2.50140422673511,92.9537027131547));
#13843=CARTESIAN_POINT('Ctrl Pts',(-1.52687742091346,2.25077736567763,93.0809693476386));
#13844=CARTESIAN_POINT('Ctrl Pts',(-2.71896989905314,-0.0674988115827291,
93.2082359821221));
#13845=CARTESIAN_POINT('Ctrl Pts',(-1.41331369599278,-2.3237680119857,93.3355026166056));
#13846=CARTESIAN_POINT('Ctrl Pts',(1.19066596354461,-2.44533595946718,93.4627692510895));
#13847=CARTESIAN_POINT('Ctrl Pts',(2.70085479964844,-0.320525725935651,
93.5900358855729));
#13848=CARTESIAN_POINT('Ctrl Pts',(1.72993617788491,2.09873157120903,93.7173025200566));
#13849=CARTESIAN_POINT('Ctrl Pts',(-0.830167301149058,2.59001460220737,
93.8445691545403));
#13850=CARTESIAN_POINT('Ctrl Pts',(-2.6276476726767,0.702012177990762,93.971835789024));
#13851=CARTESIAN_POINT('Ctrl Pts',(-2.01127142493201,-1.83088520848765,
94.0991024235075));
#13852=CARTESIAN_POINT('Ctrl Pts',(0.452734887501548,-2.68186213263241,
94.2263690579912));
#13853=CARTESIAN_POINT('Ctrl Pts',(2.50084179586903,-1.06917899042052,94.3536356924748));
#13854=CARTESIAN_POINT('Ctrl Pts',(2.2515807611881,1.52569246055347,94.4809023269583));
#13855=CARTESIAN_POINT('Ctrl Pts',(-0.0660675862559036,2.71900503214631,
94.6081689614421));
#13856=CARTESIAN_POINT('Ctrl Pts',(-2.32302375938074,1.41453672079602,94.7354355959255));
#13857=CARTESIAN_POINT('Ctrl Pts',(-2.44596234858386,-1.1893786992975,94.8627022304094));
#13858=CARTESIAN_POINT('Ctrl Pts',(-0.321947382055006,-2.70068555648289,
94.9899688648929));
#13859=CARTESIAN_POINT('Ctrl Pts',(2.09782073198627,-1.73104097344485,95.1172354993765));
#13860=CARTESIAN_POINT('Ctrl Pts',(2.5904511168555,0.828804480073396,95.2445021338601));
#13861=CARTESIAN_POINT('Ctrl Pts',(0.703395441951291,2.62727651533385,95.3717687683439));
#13862=CARTESIAN_POINT('Ctrl Pts',(-1.82982671549677,2.01223746729401,95.4990354028273));
#13863=CARTESIAN_POINT('Ctrl Pts',(-2.68209915169286,-0.451328399765236,
95.626302037311));
#13864=CARTESIAN_POINT('Ctrl Pts',(-1.07049710424441,-2.50026797207826,
95.7535686717946));
#13865=CARTESIAN_POINT('Ctrl Pts',(1.52451087035372,-2.25240527803622,95.8808353062783));
#13866=CARTESIAN_POINT('Ctrl Pts',(2.71903168804719,0.0646805712907468,
96.008101940762));
#13867=CARTESIAN_POINT('Ctrl Pts',(1.4157750712162,2.32218888596513,96.1353685752456));
#13868=CARTESIAN_POINT('Ctrl Pts',(-1.1881230839594,2.44677111654599,96.2626352097291));
#13869=CARTESIAN_POINT('Ctrl Pts',(-2.700450517374,0.322996490625344,96.3899018442128));
#13870=CARTESIAN_POINT('Ctrl Pts',(-1.73227755390183,-2.09615117838598,
96.5171684786964));
#13871=CARTESIAN_POINT('Ctrl Pts',(0.827706311696832,-2.59243844455495,
96.64443511318));
#13872=CARTESIAN_POINT('Ctrl Pts',(2.62661438719814,-0.701291050480648,
96.771719826641));
#13873=CARTESIAN_POINT('Ctrl Pts',(2.21708179584199,0.97977335842886,96.8565823286075));
#13874=CARTESIAN_POINT('Ctrl Pts',(1.70144010748552,1.54689289851004,96.8990226190793));
#13875=CARTESIAN_POINT('Ctrl Pts',(-1.07651180060961,2.20499055965285,90.7519467439103));
#13876=CARTESIAN_POINT('Ctrl Pts',(-1.81117776548521,1.84631483778521,90.7943689554048));
#13877=CARTESIAN_POINT('Ctrl Pts',(-2.88054391747525,0.341962775758166,
90.879213378394));
#13878=CARTESIAN_POINT('Ctrl Pts',(-1.84448030237179,-2.24286753756668,
91.0064800128776));
#13879=CARTESIAN_POINT('Ctrl Pts',(0.889186514994142,-2.7620929563632,91.1337466473612));
#13880=CARTESIAN_POINT('Ctrl Pts',(2.80445828551892,-0.746487008594048,
91.2610132818449));
#13881=CARTESIAN_POINT('Ctrl Pts',(2.14421290702314,1.95610910315591,91.3882799163285));
#13882=CARTESIAN_POINT('Ctrl Pts',(-0.486163295521579,2.86114059419121,
91.5155465508121));
#13883=CARTESIAN_POINT('Ctrl Pts',(-2.66974683576221,1.13811922647233,91.6428131852957));
#13884=CARTESIAN_POINT('Ctrl Pts',(-2.40089063495847,-1.63056860600089,
91.7700798197793));
#13885=CARTESIAN_POINT('Ctrl Pts',(0.073559198153165,-2.90128210971402,
91.8973464542631));
#13886=CARTESIAN_POINT('Ctrl Pts',(2.48041283950629,-1.50680357184655,92.0246130887465));
#13887=CARTESIAN_POINT('Ctrl Pts',(2.60867613123927,1.27189922896985,92.1518797232303));
#13888=CARTESIAN_POINT('Ctrl Pts',(0.340505482588885,2.8821786680068,92.2791463577138));
#13889=CARTESIAN_POINT('Ctrl Pts',(-2.24046378790063,1.84478390000535,92.4064129921973));
#13890=CARTESIAN_POINT('Ctrl Pts',(-2.76325949242661,-0.887301264587592,
92.5336796266812));
#13891=CARTESIAN_POINT('Ctrl Pts',(-0.747619797967113,-2.80427688040486,
92.6609462611647));
#13892=CARTESIAN_POINT('Ctrl Pts',(1.95481143401308,-2.14513810208465,92.7882128956484));
#13893=CARTESIAN_POINT('Ctrl Pts',(2.86147903746175,0.484605984911214,92.9154795301319));
#13894=CARTESIAN_POINT('Ctrl Pts',(1.13948360425419,2.66917254890164,93.0427461646156));
#13895=CARTESIAN_POINT('Ctrl Pts',(-1.62928456499786,2.4017362303722,93.1700127990993));
#13896=CARTESIAN_POINT('Ctrl Pts',(-2.90133027612055,-0.0720259336873552,
93.2972794335828));
#13897=CARTESIAN_POINT('Ctrl Pts',(-1.5081041600599,-2.47962233425328,93.4245460680664));
#13898=CARTESIAN_POINT('Ctrl Pts',(1.27052352068378,-2.60934380220947,93.5518127025501));
#13899=CARTESIAN_POINT('Ctrl Pts',(2.88200020322195,-0.342023276262264,
93.6790793370337));
#13900=CARTESIAN_POINT('Ctrl Pts',(1.84596240304155,2.23949277670167,93.8063459715173));
#13901=CARTESIAN_POINT('Ctrl Pts',(-0.885846336845365,2.76372599181604,
93.933612606001));
#13902=CARTESIAN_POINT('Ctrl Pts',(-2.80388309939345,0.749095893602658,
94.0608792404846));
#13903=CARTESIAN_POINT('Ctrl Pts',(-2.14616670845951,-1.95368205044725,
94.1881458749681));
#13904=CARTESIAN_POINT('Ctrl Pts',(0.483099660875866,-2.86173370455381,
94.3154125094519));
#13905=CARTESIAN_POINT('Ctrl Pts',(2.66857239599058,-1.14088845800733,94.4426791439354));
#13906=CARTESIAN_POINT('Ctrl Pts',(2.40259350934356,1.6280201297536,94.5699457784191));
#13907=CARTESIAN_POINT('Ctrl Pts',(-0.0704987165695354,2.9013677655782,
94.6972124129027));
#13908=CARTESIAN_POINT('Ctrl Pts',(-2.47882816488178,1.50940921271655,94.8244790473864));
#13909=CARTESIAN_POINT('Ctrl Pts',(-2.61001220302903,-1.26914992006584,
94.9517456818698));
#13910=CARTESIAN_POINT('Ctrl Pts',(-0.343540282369155,-2.88181960897544,
95.0790123163536));
#13911=CARTESIAN_POINT('Ctrl Pts',(2.23852084780516,-1.84714129686014,95.2062789508372));
#13912=CARTESIAN_POINT('Ctrl Pts',(2.76419178335165,0.884392111828334,95.3335455853208));
#13913=CARTESIAN_POINT('Ctrl Pts',(0.750571932601818,2.80348704865511,95.4608122198045));
#13914=CARTESIAN_POINT('Ctrl Pts',(-1.9525525646951,2.14719754295085,95.5880788542881));
#13915=CARTESIAN_POINT('Ctrl Pts',(-2.86198662040122,-0.481598840490258,
95.7153454887717));
#13916=CARTESIAN_POINT('Ctrl Pts',(-1.14229497727256,-2.66796008603529,
95.8426121232553));
#13917=CARTESIAN_POINT('Ctrl Pts',(1.62675929070508,-2.40347332625343,95.969878757739));
#13918=CARTESIAN_POINT('Ctrl Pts',(2.90139620928121,0.0690186749871554,
96.0971453922227));
#13919=CARTESIAN_POINT('Ctrl Pts',(1.510730618874,2.477937296793,96.2244120267062));
#13920=CARTESIAN_POINT('Ctrl Pts',(-1.26781009103836,2.61087521478053,96.3516786611899));
#13921=CARTESIAN_POINT('Ctrl Pts',(-2.88156880587425,0.344659754290898,
96.4789452956735));
#13922=CARTESIAN_POINT('Ctrl Pts',(-1.84846081434358,-2.23673931781844,
96.6062119301572));
#13923=CARTESIAN_POINT('Ctrl Pts',(0.883220289676016,-2.76631240043719,
96.7334785646408));
#13924=CARTESIAN_POINT('Ctrl Pts',(2.80278051181281,-0.748326400318174,
96.8607632781017));
#13925=CARTESIAN_POINT('Ctrl Pts',(2.3657807102433,1.04548642099196,96.9456257800682));
#13926=CARTESIAN_POINT('Ctrl Pts',(1.81555511098988,1.65064247380082,96.98806607054));
#13927=CARTESIAN_POINT('Ctrl Pts',(0.588712386787453,-2.38292909182934,
96.7230113585668));
#13928=CARTESIAN_POINT('Ctrl Pts',(0.640648769308371,-2.3652933144126,96.7230113585668));
#13929=CARTESIAN_POINT('Ctrl Pts',(0.691875067436002,-2.34581391031218,
96.7230113585668));
#13930=CARTESIAN_POINT('Ctrl Pts',(0.742296016079015,-2.32446461360961,
96.7230113585668));
#13931=CARTESIAN_POINT('Ctrl Pts',(0.820739821153515,-2.2912498464526,96.7230113585668));
#13932=CARTESIAN_POINT('Ctrl Pts',(0.897236129890821,-2.25351082281703,
96.7230113585668));
#13933=CARTESIAN_POINT('Ctrl Pts',(0.971544835524987,-2.21156500778445,
96.7230113585668));
#13934=CARTESIAN_POINT('Ctrl Pts',(1.03217330020216,-2.17734142195619,96.7230113585668));
#13935=CARTESIAN_POINT('Ctrl Pts',(1.09134509111778,-2.14031633100486,96.7230113585668));
#13936=CARTESIAN_POINT('Ctrl Pts',(1.14891121002181,-2.10064528356617,96.7230113585668));
#13937=CARTESIAN_POINT('Ctrl Pts',(1.16159513936322,-2.09190429542607,96.7230113585668));
#13938=CARTESIAN_POINT('Ctrl Pts',(1.17419734893583,-2.08303729003666,96.7230113585668));
#13939=CARTESIAN_POINT('Ctrl Pts',(1.18671008065498,-2.07405069777297,96.7230113585668));
#13940=CARTESIAN_POINT('Ctrl Pts',(1.2556958568937,-2.02450539807606,96.7230113585668));
#13941=CARTESIAN_POINT('Ctrl Pts',(1.32202432452181,-1.97128734189988,96.7230113585668));
#13942=CARTESIAN_POINT('Ctrl Pts',(1.38545426454246,-1.91470942721314,96.7230113585668));
#13943=CARTESIAN_POINT('Ctrl Pts',(1.43441942286438,-1.87103373479946,96.7230113585668));
#13944=CARTESIAN_POINT('Ctrl Pts',(1.48165667196868,-1.82535488812884,96.7230113585668));
#13945=CARTESIAN_POINT('Ctrl Pts',(1.52703736438344,-1.7778050599483,96.7230113585668));
#13946=CARTESIAN_POINT('Ctrl Pts',(1.54858651511599,-1.75522588893425,96.7230113585668));
#13947=CARTESIAN_POINT('Ctrl Pts',(1.56971679742231,-1.73222471822232,96.7230113585668));
#13948=CARTESIAN_POINT('Ctrl Pts',(1.59041304366888,-1.70881516364333,96.7230113585668));
#13949=CARTESIAN_POINT('Ctrl Pts',(1.60045213541326,-1.69745993220119,96.7230113585668));
#13950=CARTESIAN_POINT('Ctrl Pts',(1.61039045013747,-1.68600700476021,96.7230113585668));
#13951=CARTESIAN_POINT('Ctrl Pts',(1.62022185084907,-1.67446300273117,96.7230113585668));
#13952=CARTESIAN_POINT('Ctrl Pts',(1.67412442902213,-1.61117075271984,96.7230113585668));
#13953=CARTESIAN_POINT('Ctrl Pts',(1.72466397502101,-1.54532438173906,96.7230113585668));
#13954=CARTESIAN_POINT('Ctrl Pts',(1.77161894887438,-1.47721544158816,96.7230113585668));
#13955=CARTESIAN_POINT('Ctrl Pts',(1.81810231493719,-1.40979057607613,96.7230113585668));
#13956=CARTESIAN_POINT('Ctrl Pts',(1.86107318675472,-1.34014747392538,96.7230113585667));
#13957=CARTESIAN_POINT('Ctrl Pts',(1.90027066793302,-1.26854810370225,96.7230113585667));
#13958=CARTESIAN_POINT('Ctrl Pts',(1.93827854866182,-1.19912169562974,96.7230113585667));
#13959=CARTESIAN_POINT('Ctrl Pts',(1.97273879647841,-1.1278551884302,96.7230113585667));
#13960=CARTESIAN_POINT('Ctrl Pts',(2.00336580355094,-1.05497981877367,96.7230113585667));
#13961=CARTESIAN_POINT('Ctrl Pts',(2.02129404247609,-1.01232050714498,96.7230113585667));
#13962=CARTESIAN_POINT('Ctrl Pts',(2.03790785886586,-0.969109813993785,
96.7230113585668));
#13963=CARTESIAN_POINT('Ctrl Pts',(2.05314159279707,-0.925394393548234,
96.7230113585668));
#13964=CARTESIAN_POINT('Ctrl Pts',(2.05752593699301,-0.912812878683333,
96.7230113585668));
#13965=CARTESIAN_POINT('Ctrl Pts',(2.06179609056006,-0.90018878324672,96.7230113585667));
#13966=CARTESIAN_POINT('Ctrl Pts',(2.06594555589405,-0.887538783166725,
96.7230113585667));
#13967=CARTESIAN_POINT('Ctrl Pts',(2.09030106369674,-0.813288933884062,
96.7230113585667));
#13968=CARTESIAN_POINT('Ctrl Pts',(2.11054754703649,-0.738021766380488,
96.7230113585668));
#13969=CARTESIAN_POINT('Ctrl Pts',(2.1264523557256,-0.661972017543704,96.7230113585668));
#13970=CARTESIAN_POINT('Ctrl Pts',(2.13251522995639,-0.632982039009962,
96.7230113585668));
#13971=CARTESIAN_POINT('Ctrl Pts',(2.13794668381121,-0.603878262914742,
96.7230113585667));
#13972=CARTESIAN_POINT('Ctrl Pts',(2.14273181896565,-0.574673529019169,
96.7230113585667));
#13973=CARTESIAN_POINT('Ctrl Pts',(2.15558851779652,-0.496206264038638,
96.7230113585667));
#13974=CARTESIAN_POINT('Ctrl Pts',(2.16378320115503,-0.417009388046162,
96.7230113585668));
#13975=CARTESIAN_POINT('Ctrl Pts',(2.16743223057129,-0.33743940379413,96.7230113585668));
#13976=CARTESIAN_POINT('Ctrl Pts',(2.17098140797991,-0.260046771864714,
96.7230113585668));
#13977=CARTESIAN_POINT('Ctrl Pts',(2.17022968718329,-0.182300337705529,
96.7230113585668));
#13978=CARTESIAN_POINT('Ctrl Pts',(2.16523998757234,-0.104545110509807,
96.7230113585668));
#13979=CARTESIAN_POINT('Ctrl Pts',(2.16444474155328,-0.0921526741489186,
96.7230113585668));
#13980=CARTESIAN_POINT('Ctrl Pts',(2.16354155389744,-0.0797575534964672,
96.7230113585668));
#13981=CARTESIAN_POINT('Ctrl Pts',(2.1625312776458,-0.0673695075572312,
96.7230113585668));
#13982=CARTESIAN_POINT('Ctrl Pts',(2.1562180590047,0.0100434202668876,96.7230113585668));
#13983=CARTESIAN_POINT('Ctrl Pts',(2.14574427085824,0.0869961031253285,
96.7230113585668));
#13984=CARTESIAN_POINT('Ctrl Pts',(2.13125086339959,0.163162923078114,96.7230113585668));
#13985=CARTESIAN_POINT('Ctrl Pts',(2.11677422416584,0.239241621423175,96.7230113585668));
#13986=CARTESIAN_POINT('Ctrl Pts',(2.09828678062113,0.314537217629474,96.7230113585668));
#13987=CARTESIAN_POINT('Ctrl Pts',(2.07588093305262,0.388707135189438,96.7230113585668));
#13988=CARTESIAN_POINT('Ctrl Pts',(2.05365575074666,0.462278997818072,96.7230113585668));
#13989=CARTESIAN_POINT('Ctrl Pts',(2.02757460817981,0.534744112225099,96.7230113585668));
#13990=CARTESIAN_POINT('Ctrl Pts',(1.99768768671817,0.605737007823448,96.7230113585668));
#13991=CARTESIAN_POINT('Ctrl Pts',(1.98597215240563,0.633565892956258,96.7230113585668));
#13992=CARTESIAN_POINT('Ctrl Pts',(1.97367142411387,0.661168148916436,96.7230113585668));
#13993=CARTESIAN_POINT('Ctrl Pts',(1.96078707526267,0.688520011253182,96.7230113585668));
#13994=CARTESIAN_POINT('Ctrl Pts',(1.95276721707462,0.705545167871723,96.7230113585668));
#13995=CARTESIAN_POINT('Ctrl Pts',(1.94451794942827,0.722479472898389,96.7230113585668));
#13996=CARTESIAN_POINT('Ctrl Pts',(1.93605669336428,0.739283797803819,96.7230113585668));
#13997=CARTESIAN_POINT('Ctrl Pts',(1.90242108599403,0.806085188798996,96.7230113585668));
#13998=CARTESIAN_POINT('Ctrl Pts',(1.86540482271834,0.870913728227497,96.7230113585667));
#13999=CARTESIAN_POINT('Ctrl Pts',(1.8250950839614,0.933459813271843,96.7230113585667));
#14000=CARTESIAN_POINT('Ctrl Pts',(1.78524429298128,0.995293777931269,96.7230113585667));
#14001=CARTESIAN_POINT('Ctrl Pts',(1.74217409759157,1.05489768041583,96.7230113585667));
#14002=CARTESIAN_POINT('Ctrl Pts',(1.69593353228868,1.11193673353134,96.7230113585667));
#14003=CARTESIAN_POINT('Ctrl Pts',(1.65129120780821,1.16700431111312,96.7230113585667));
#14004=CARTESIAN_POINT('Ctrl Pts',(1.60369337036815,1.21968169051598,96.7230113585667));
#14005=CARTESIAN_POINT('Ctrl Pts',(1.55315866977046,1.26962629746061,96.7230113585667));
#14006=CARTESIAN_POINT('Ctrl Pts',(1.52831927675166,1.29417564090965,96.7230113585667));
#14007=CARTESIAN_POINT('Ctrl Pts',(1.50276997933335,1.31806405778729,96.7230113585667));
#14008=CARTESIAN_POINT('Ctrl Pts',(1.47651116554366,1.34124656216704,96.7230113585667));
#14009=CARTESIAN_POINT('Ctrl Pts',(-1.1629311539782,-1.62480320830708,90.7500736540522));
#14010=CARTESIAN_POINT('Ctrl Pts',(-1.20248717512367,-1.60291707496938,
90.7500736540522));
#14011=CARTESIAN_POINT('Ctrl Pts',(-1.24117742673991,-1.5796333799921,90.7500736540522));
#14012=CARTESIAN_POINT('Ctrl Pts',(-1.27891854248392,-1.5549680498462,90.7500736540522));
#14013=CARTESIAN_POINT('Ctrl Pts',(-1.3391412895418,-1.51561007355979,90.7500736540522));
#14014=CARTESIAN_POINT('Ctrl Pts',(-1.39694873666562,-1.47273701788695,
90.7500736540522));
#14015=CARTESIAN_POINT('Ctrl Pts',(-1.45225791381737,-1.42669773153816,
90.7500736540522));
#14016=CARTESIAN_POINT('Ctrl Pts',(-1.48252910851924,-1.40150002886441,
90.7500736540522));
#14017=CARTESIAN_POINT('Ctrl Pts',(-1.51205165542062,-1.37535297886323,
90.7500736540522));
#14018=CARTESIAN_POINT('Ctrl Pts',(-1.5408093008143,-1.34830778980114,90.7500736540522));
#14019=CARTESIAN_POINT('Ctrl Pts',(-1.55479063378575,-1.33515901533173,
90.7500736540522));
#14020=CARTESIAN_POINT('Ctrl Pts',(-1.56859113601269,-1.32179788964324,
90.7500736540522));
#14021=CARTESIAN_POINT('Ctrl Pts',(-1.58220874619757,-1.30822998007715,
90.7500736540522));
#14022=CARTESIAN_POINT('Ctrl Pts',(-1.59343008164899,-1.29704959948551,
90.7500736540522));
#14023=CARTESIAN_POINT('Ctrl Pts',(-1.60452061623741,-1.2857353417468,90.7500736540522));
#14024=CARTESIAN_POINT('Ctrl Pts',(-1.61547660352134,-1.27429395107632,
90.7500736540522));
#14025=CARTESIAN_POINT('Ctrl Pts',(-1.66744198904932,-1.22002624687413,
90.7500736540522));
#14026=CARTESIAN_POINT('Ctrl Pts',(-1.71640398877985,-1.16288084511768,
90.7500736540522));
#14027=CARTESIAN_POINT('Ctrl Pts',(-1.76226853571781,-1.10322863632069,
90.7500736540522));
#14028=CARTESIAN_POINT('Ctrl Pts',(-1.79953220669005,-1.05476287289812,
90.7500736540522));
#14029=CARTESIAN_POINT('Ctrl Pts',(-1.83475096252,-1.00464114381801,90.7500736540523));
#14030=CARTESIAN_POINT('Ctrl Pts',(-1.86786104451265,-0.953040921544573,
90.7500736540523));
#14031=CARTESIAN_POINT('Ctrl Pts',(-1.88146828181041,-0.931834798610553,
90.7500736540523));
#14032=CARTESIAN_POINT('Ctrl Pts',(-1.89471921467165,-0.910378765130967,
90.7500736540522));
#14033=CARTESIAN_POINT('Ctrl Pts',(-1.90760870916851,-0.888684374343241,
90.7500736540522));
#14034=CARTESIAN_POINT('Ctrl Pts',(-1.91577328640956,-0.87494252206757,
90.7500736540522));
#14035=CARTESIAN_POINT('Ctrl Pts',(-1.92379338532837,-0.86110380603922,
90.7500736540523));
#14036=CARTESIAN_POINT('Ctrl Pts',(-1.93165776304693,-0.847189230573697,
90.7500736540523));
#14037=CARTESIAN_POINT('Ctrl Pts',(-1.97012662979234,-0.779125619114782,
90.7500736540523));
#14038=CARTESIAN_POINT('Ctrl Pts',(-2.00493023271791,-0.709154461979746,
90.7500736540523));
#14039=CARTESIAN_POINT('Ctrl Pts',(-2.03597045608216,-0.637659028599459,
90.7500736540523));
#14040=CARTESIAN_POINT('Ctrl Pts',(-2.06739142995637,-0.565286606597039,
90.7500736540523));
#14041=CARTESIAN_POINT('Ctrl Pts',(-2.0949567808205,-0.491351478981031,
90.7500736540523));
#14042=CARTESIAN_POINT('Ctrl Pts',(-2.11852959809477,-0.416210774009595,
90.7500736540523));
#14043=CARTESIAN_POINT('Ctrl Pts',(-2.14196667005475,-0.341502770759492,
90.7500736540523));
#14044=CARTESIAN_POINT('Ctrl Pts',(-2.16145761271948,-0.265602104107118,
90.7500736540523));
#14045=CARTESIAN_POINT('Ctrl Pts',(-2.17682448455395,-0.18883326108786,
90.7500736540523));
#14046=CARTESIAN_POINT('Ctrl Pts',(-2.18114611784962,-0.16724351975103,
90.7500736540523));
#14047=CARTESIAN_POINT('Ctrl Pts',(-2.1851412830939,-0.145584999209621,
90.7500736540523));
#14048=CARTESIAN_POINT('Ctrl Pts',(-2.18880530501091,-0.123864692850796,
90.7500736540523));
#14049=CARTESIAN_POINT('Ctrl Pts',(-2.19098529876454,-0.110941699140181,
90.7500736540523));
#14050=CARTESIAN_POINT('Ctrl Pts',(-2.19304836677221,-0.0979947967337072,
90.7500736540523));
#14051=CARTESIAN_POINT('Ctrl Pts',(-2.19499250099196,-0.085031936846214,
90.7500736540523));
#14052=CARTESIAN_POINT('Ctrl Pts',(-2.20701790455726,-0.00485042472448606,
90.7500736540523));
#14053=CARTESIAN_POINT('Ctrl Pts',(-2.2144573386233,0.0756695034371889,
90.7500736540523));
#14054=CARTESIAN_POINT('Ctrl Pts',(-2.21718406235607,0.156150190113027,
90.7500736540523));
#14055=CARTESIAN_POINT('Ctrl Pts',(-2.21836944509456,0.191137385779644,
90.7500736540523));
#14056=CARTESIAN_POINT('Ctrl Pts',(-2.21866364274063,0.226117562255175,
90.7500736540523));
#14057=CARTESIAN_POINT('Ctrl Pts',(-2.21805357014175,0.261061209453445,
90.7500736540523));
#14058=CARTESIAN_POINT('Ctrl Pts',(-2.21668480419082,0.339461181152025,
90.7500736540523));
#14059=CARTESIAN_POINT('Ctrl Pts',(-2.21076796745135,0.417676800779223,
90.7500736540523));
#14060=CARTESIAN_POINT('Ctrl Pts',(-2.20054345997488,0.49544826966194,90.7500736540523));
#14061=CARTESIAN_POINT('Ctrl Pts',(-2.19031895249841,0.573219738544656,
90.7500736540523));
#14062=CARTESIAN_POINT('Ctrl Pts',(-2.17578648103929,0.650547822033016,
90.7500736540523));
#14063=CARTESIAN_POINT('Ctrl Pts',(-2.15713417814691,0.727175031660327,
90.7500736540523));
#14064=CARTESIAN_POINT('Ctrl Pts',(-2.1539803082068,0.740131729523996,90.7500736540523));
#14065=CARTESIAN_POINT('Ctrl Pts',(-2.15070853499987,0.753068378664176,
90.7500736540523));
#14066=CARTESIAN_POINT('Ctrl Pts',(-2.14731962968966,0.765983716177013,
90.7500736540523));
#14067=CARTESIAN_POINT('Ctrl Pts',(-2.14412530405667,0.778157497944161,
90.7500736540523));
#14068=CARTESIAN_POINT('Ctrl Pts',(-2.14082936994079,0.790302951605743,
90.7500736540523));
#14069=CARTESIAN_POINT('Ctrl Pts',(-2.13743320332618,0.802418155946092,
90.7500736540523));
#14070=CARTESIAN_POINT('Ctrl Pts',(-2.11559292525712,0.88032936045494,90.7500736540523));
#14071=CARTESIAN_POINT('Ctrl Pts',(-2.08960869205439,0.957000970977793,
90.7500736540522));
#14072=CARTESIAN_POINT('Ctrl Pts',(-2.05975308903368,1.0321622444044,90.7500736540522));
#14073=CARTESIAN_POINT('Ctrl Pts',(-2.02936458120719,1.10866510198154,90.7500736540522));
#14074=CARTESIAN_POINT('Ctrl Pts',(-1.99496506341364,1.18360404711025,90.7500736540523));
#14075=CARTESIAN_POINT('Ctrl Pts',(-1.9567873698184,1.25669491216257,90.7500736540523));
#14076=CARTESIAN_POINT('Ctrl Pts',(-1.91822311031008,1.33052585432081,90.7500736540523));
#14077=CARTESIAN_POINT('Ctrl Pts',(-1.87580347456082,1.40247202242494,90.7500736540523));
#14078=CARTESIAN_POINT('Ctrl Pts',(-1.82971715604818,1.47222861375008,90.7500736540523));
#14079=CARTESIAN_POINT('Ctrl Pts',(-1.81119809279695,1.50025920435988,90.7500736540523));
#14080=CARTESIAN_POINT('Ctrl Pts',(-1.79208641832787,1.52793603129552,90.7500736540522));
#14081=CARTESIAN_POINT('Ctrl Pts',(-1.77239225197708,1.55523825579694,90.7500736540522));
#14082=CARTESIAN_POINT('Ctrl Pts',(-1.76263940974474,1.56875872086315,90.7500736540522));
#14083=CARTESIAN_POINT('Ctrl Pts',(-1.75274156406399,1.58218996914953,90.7500736540522));
#14084=CARTESIAN_POINT('Ctrl Pts',(-1.74271568305835,1.59550888248852,90.7500736540522));
#14085=CARTESIAN_POINT('Ctrl Pts',(-1.69105993064107,1.66413113020107,90.7500736540522));
#14086=CARTESIAN_POINT('Ctrl Pts',(-1.63593306559914,1.72988154427594,90.7500736540522));
#14087=CARTESIAN_POINT('Ctrl Pts',(-1.5775910963695,1.79246237937079,90.7500736540522));
#14088=CARTESIAN_POINT('Ctrl Pts',(-1.51916579161454,1.85513260477654,90.7500736540522));
#14089=CARTESIAN_POINT('Ctrl Pts',(-1.45751575777673,1.91462512805355,90.7500736540522));
#14090=CARTESIAN_POINT('Ctrl Pts',(-1.39284891655045,1.9706235418493,90.7500736540522));
#14091=CARTESIAN_POINT('Ctrl Pts',(-1.3295666745946,2.02542295842457,90.7500736540522));
#14092=CARTESIAN_POINT('Ctrl Pts',(-1.2633948711054,2.07687707547168,90.7500736540522));
#14093=CARTESIAN_POINT('Ctrl Pts',(-1.19448888753409,2.12466016003287,90.7500736540522));
#14094=CARTESIAN_POINT('Ctrl Pts',(-1.15555458977215,2.15165927891728,90.7500736540522));
#14095=CARTESIAN_POINT('Ctrl Pts',(-1.11574669177119,2.17748577160815,90.7500736540522));
#14096=CARTESIAN_POINT('Ctrl Pts',(-1.07508846035166,2.2020751695659,90.7500736540522));
#14097=CARTESIAN_POINT('Origin',(-5.69858952725515E-16,8.58067791224701E-17,
90.7500736540522));
#14098=CARTESIAN_POINT('',(-2.4505,-3.00099698131059E-16,90.7500736540522));
#14099=CARTESIAN_POINT('Origin',(0.,0.,90.7500736540522));
#14100=CARTESIAN_POINT('',(1.11860366144128,2.18029266352253,90.7500736540522));
#14101=CARTESIAN_POINT('Origin',(0.,0.,90.7500736540522));
#14102=CARTESIAN_POINT('Ctrl Pts',(1.11860366144127,2.18029266352252,90.7500736540522));
#14103=CARTESIAN_POINT('Ctrl Pts',(1.15162264457275,2.15955585985248,90.7500736540522));
#14104=CARTESIAN_POINT('Ctrl Pts',(1.18407930231287,2.13798223312585,90.7500736540523));
#14105=CARTESIAN_POINT('Ctrl Pts',(1.2159377932849,2.11556938451728,90.7500736540523));
#14106=CARTESIAN_POINT('Ctrl Pts',(1.28560972406618,2.06655430598646,90.7500736540523));
#14107=CARTESIAN_POINT('Ctrl Pts',(1.35242359596798,2.01352759821736,90.7500736540523));
#14108=CARTESIAN_POINT('Ctrl Pts',(1.41621167348851,1.95685023476083,90.7500736540523));
#14109=CARTESIAN_POINT('Ctrl Pts',(1.4485350295639,1.92813009344868,90.7500736540523));
#14110=CARTESIAN_POINT('Ctrl Pts',(1.48008078664681,1.89847201623414,90.7500736540522));
#14111=CARTESIAN_POINT('Ctrl Pts',(1.51082285430447,1.8679203368343,90.7500736540522));
#14112=CARTESIAN_POINT('Ctrl Pts',(1.52957938642694,1.84927996552161,90.7500736540522));
#14113=CARTESIAN_POINT('Ctrl Pts',(1.54803668440887,1.83030691799242,90.7500736540522));
#14114=CARTESIAN_POINT('Ctrl Pts',(1.56618825539262,1.81101104547671,90.7500736540522));
#14115=CARTESIAN_POINT('Ctrl Pts',(1.57674283195666,1.79979109299882,90.7500736540522));
#14116=CARTESIAN_POINT('Ctrl Pts',(1.58719094483532,1.78846519805228,90.7500736540522));
#14117=CARTESIAN_POINT('Ctrl Pts',(1.59752636698703,1.7770412829028,90.7500736540522));
#14118=CARTESIAN_POINT('Ctrl Pts',(1.65450684340916,1.71405980829358,90.7500736540522));
#14119=CARTESIAN_POINT('Ctrl Pts',(1.70811520307835,1.64804892541984,90.7500736540522));
#14120=CARTESIAN_POINT('Ctrl Pts',(1.7581816725158,1.57936535303345,90.7500736540522));
#14121=CARTESIAN_POINT('Ctrl Pts',(1.79683292035112,1.52634172647561,90.7500736540522));
#14122=CARTESIAN_POINT('Ctrl Pts',(1.83337245026146,1.47172442149015,90.7500736540522));
#14123=CARTESIAN_POINT('Ctrl Pts',(1.86770238229061,1.41566979012823,90.7500736540522));
#14124=CARTESIAN_POINT('Ctrl Pts',(1.88400353449563,1.38905292771059,90.7500736540522));
#14125=CARTESIAN_POINT('Ctrl Pts',(1.89980622399855,1.36211192267649,90.7500736540522));
#14126=CARTESIAN_POINT('Ctrl Pts',(1.91509849671254,1.33486328413342,90.7500736540522));
#14127=CARTESIAN_POINT('Ctrl Pts',(1.9225163087319,1.32164580611193,90.7500736540522));
#14128=CARTESIAN_POINT('Ctrl Pts',(1.92981500217531,1.30835408931338,90.7500736540522));
#14129=CARTESIAN_POINT('Ctrl Pts',(1.93698997498754,1.29499590064715,90.7500736540522));
#14130=CARTESIAN_POINT('Ctrl Pts',(1.97632810621595,1.22175713131972,90.7500736540522));
#14131=CARTESIAN_POINT('Ctrl Pts',(2.011840092034,1.14673115001634,90.7500736540522));
#14132=CARTESIAN_POINT('Ctrl Pts',(2.04337087962439,1.0702496833273,90.7500736540522));
#14133=CARTESIAN_POINT('Ctrl Pts',(2.07458497279001,0.994536394535134,90.7500736540522));
#14134=CARTESIAN_POINT('Ctrl Pts',(2.1018976767583,0.917395750779118,90.7500736540522));
#14135=CARTESIAN_POINT('Ctrl Pts',(2.12510922745775,0.839138863226887,90.7500736540522));
#14136=CARTESIAN_POINT('Ctrl Pts',(2.14761632748849,0.763257005136517,90.7500736540522));
#14137=CARTESIAN_POINT('Ctrl Pts',(2.16626745954812,0.686324834641116,90.7500736540522));
#14138=CARTESIAN_POINT('Ctrl Pts',(2.18083222156942,0.608628635176532,90.7500736540522));
#14139=CARTESIAN_POINT('Ctrl Pts',(2.1893580477943,0.563147336271684,90.7500736540522));
#14140=CARTESIAN_POINT('Ctrl Pts',(2.19648271621353,0.517404343444855,90.7500736540522));
#14141=CARTESIAN_POINT('Ctrl Pts',(2.20215188602963,0.471459112307776,90.7500736540522));
#14142=CARTESIAN_POINT('Ctrl Pts',(2.20378351406345,0.458235742824217,90.7500736540522));
#14143=CARTESIAN_POINT('Ctrl Pts',(2.20529453685117,0.444994839301754,90.7500736540522));
#14144=CARTESIAN_POINT('Ctrl Pts',(2.20668212071864,0.431754073468555,90.7500736540522));
#14145=CARTESIAN_POINT('Ctrl Pts',(2.21482655469238,0.354037298563444,90.7500736540522));
#14146=CARTESIAN_POINT('Ctrl Pts',(2.21873982537425,0.276192904866269,90.7500736540522));
#14147=CARTESIAN_POINT('Ctrl Pts',(2.21824403489587,0.198499425861476,90.7500736540522));
#14148=CARTESIAN_POINT('Ctrl Pts',(2.21805504044083,0.168882808833148,90.7500736540522));
#14149=CARTESIAN_POINT('Ctrl Pts',(2.2172248263468,0.139288154592789,90.7500736540522));
#14150=CARTESIAN_POINT('Ctrl Pts',(2.2157415379887,0.109731156930863,90.7500736540522));
#14151=CARTESIAN_POINT('Ctrl Pts',(2.21175624551703,0.0303175488993252,
90.7500736540522));
#14152=CARTESIAN_POINT('Ctrl Pts',(2.20305993064706,-0.0488257888431539,
90.7500736540522));
#14153=CARTESIAN_POINT('Ctrl Pts',(2.18984154198201,-0.127374924856007,
90.7500736540522));
#14154=CARTESIAN_POINT('Ctrl Pts',(2.17698486180796,-0.20377463931855,90.7500736540522));
#14155=CARTESIAN_POINT('Ctrl Pts',(2.15984942904707,-0.279612912181562,
90.7500736540522));
#14156=CARTESIAN_POINT('Ctrl Pts',(2.13856952809271,-0.354565773154105,
90.7500736540522));
#14157=CARTESIAN_POINT('Ctrl Pts',(2.13517799014349,-0.3665115746377,90.7500736540522));
#14158=CARTESIAN_POINT('Ctrl Pts',(2.1316803732889,-0.378437229566964,90.7500736540522));
#14159=CARTESIAN_POINT('Ctrl Pts',(2.12807957002442,-0.390333378570073,
90.7500736540522));
#14160=CARTESIAN_POINT('Ctrl Pts',(2.10555064548884,-0.464763283085853,
90.7500736540522));
#14161=CARTESIAN_POINT('Ctrl Pts',(2.07904216588284,-0.537862381076858,
90.7500736540522));
#14162=CARTESIAN_POINT('Ctrl Pts',(2.04876132870682,-0.609341044688673,
90.7500736540522));
#14163=CARTESIAN_POINT('Ctrl Pts',(2.01842212874393,-0.680957475099535,
90.7500736540522));
#14164=CARTESIAN_POINT('Ctrl Pts',(1.98429535798103,-0.750948067942242,
90.7500736540522));
#14165=CARTESIAN_POINT('Ctrl Pts',(1.94654558957243,-0.818993232114188,
90.7500736540522));
#14166=CARTESIAN_POINT('Ctrl Pts',(1.9095059907965,-0.88575829282372,90.7500736540522));
#14167=CARTESIAN_POINT('Ctrl Pts',(1.86897771992724,-0.950651078774011,
90.7500736540522));
#14168=CARTESIAN_POINT('Ctrl Pts',(1.8250843907989,-1.01333162280846,90.7500736540522));
#14169=CARTESIAN_POINT('Ctrl Pts',(1.80772089155411,-1.03812704390362,90.7500736540522));
#14170=CARTESIAN_POINT('Ctrl Pts',(1.78983050709486,-1.06257580205391,90.7500736540522));
#14171=CARTESIAN_POINT('Ctrl Pts',(1.77141983903051,-1.08665482731573,90.7500736540522));
#14172=CARTESIAN_POINT('Ctrl Pts',(1.75998908115404,-1.10160493704056,90.7500736540522));
#14173=CARTESIAN_POINT('Ctrl Pts',(1.74835324490105,-1.11641784806647,90.7500736540522));
#14174=CARTESIAN_POINT('Ctrl Pts',(1.73653761305467,-1.13105898801412,90.7500736540522));
#14175=CARTESIAN_POINT('Ctrl Pts',(1.6894484845429,-1.18940868352909,90.7500736540522));
#14176=CARTESIAN_POINT('Ctrl Pts',(1.63945635267561,-1.24510343119323,90.7500736540522));
#14177=CARTESIAN_POINT('Ctrl Pts',(1.58671285136659,-1.29785677787551,90.7500736540522));
#14178=CARTESIAN_POINT('Ctrl Pts',(1.5348340863669,-1.34974522683233,90.7500736540522));
#14179=CARTESIAN_POINT('Ctrl Pts',(1.48029277358304,-1.39878848761766,90.7500736540522));
#14180=CARTESIAN_POINT('Ctrl Pts',(1.4232065330979,-1.44467201634083,90.7500736540522));
#14181=CARTESIAN_POINT('Ctrl Pts',(1.36795223109561,-1.48908310965255,90.7500736540522));
#14182=CARTESIAN_POINT('Ctrl Pts',(1.31031313664948,-1.53053432787586,90.7500736540522));
#14183=CARTESIAN_POINT('Ctrl Pts',(1.2503797473084,-1.56869474102025,90.7500736540522));
#14184=CARTESIAN_POINT('Ctrl Pts',(1.22092070607232,-1.58745171766992,90.7500736540522));
#14185=CARTESIAN_POINT('Ctrl Pts',(1.19090716214411,-1.60541289253108,90.7500736540522));
#14186=CARTESIAN_POINT('Ctrl Pts',(1.16034898466942,-1.62253437445148,90.7500736540522));
#14187=CARTESIAN_POINT('Ctrl Pts',(1.42641864629319,-1.99638045030102,90.4850961099509));
#14188=CARTESIAN_POINT('Ctrl Pts',(2.09188384541137,-1.52093832304627,90.5275363992458));
#14189=CARTESIAN_POINT('Ctrl Pts',(2.89741194200073,0.140230266537244,90.6123989000352));
#14190=CARTESIAN_POINT('Ctrl Pts',(1.44681938588662,2.51760976119924,90.7396836123194));
#14191=CARTESIAN_POINT('Ctrl Pts',(-1.3349513413323,2.57619747619588,90.8669502468028));
#14192=CARTESIAN_POINT('Ctrl Pts',(-2.88927286053599,0.270948746763703,
90.9942168812865));
#14193=CARTESIAN_POINT('Ctrl Pts',(-1.78994692638796,-2.28455322460687,
91.12148351577));
#14194=CARTESIAN_POINT('Ctrl Pts',(0.953961383261563,-2.74071497093679,
91.2487501502538));
#14195=CARTESIAN_POINT('Ctrl Pts',(2.82139223301607,-0.679478173895668,
91.3760167847374));
#14196=CARTESIAN_POINT('Ctrl Pts',(2.09705047335778,2.00611323769679,91.5032834192211));
#14197=CARTESIAN_POINT('Ctrl Pts',(-0.553753233031221,2.84873431719668,
91.6305500537047));
#14198=CARTESIAN_POINT('Ctrl Pts',(-2.69584252699719,1.07443894056368,91.7578166881883));
#14199=CARTESIAN_POINT('Ctrl Pts',(-2.36143656052974,-1.68689575431721,
91.885083322672));
#14200=CARTESIAN_POINT('Ctrl Pts',(0.142278221441695,-2.89857479605069,
92.0123499571555));
#14201=CARTESIAN_POINT('Ctrl Pts',(2.51528897469708,-1.44751790783786,92.1396165916392));
#14202=CARTESIAN_POINT('Ctrl Pts',(2.57766098092973,1.33328598602465,92.2668832261228));
#14203=CARTESIAN_POINT('Ctrl Pts',(0.272095583979841,2.88928179142881,92.3941498606065));
#14204=CARTESIAN_POINT('Ctrl Pts',(-2.28342689430216,1.79107451910037,92.52141649509));
#14205=CARTESIAN_POINT('Ctrl Pts',(-2.74130709999466,-0.952481874254109,
92.6486831295738));
#14206=CARTESIAN_POINT('Ctrl Pts',(-0.680918780824363,-2.82105223071625,
92.7759497640573));
#14207=CARTESIAN_POINT('Ctrl Pts',(2.00498727946868,-2.09809728512521,92.9032163985409));
#14208=CARTESIAN_POINT('Ctrl Pts',(2.8490361412242,0.552249279642321,93.0304830330245));
#14209=CARTESIAN_POINT('Ctrl Pts',(1.0758525501431,2.6952787356818,93.1577496675082));
#14210=CARTESIAN_POINT('Ctrl Pts',(-1.68564991556116,2.36232312597231,93.2850163019919));
#14211=CARTESIAN_POINT('Ctrl Pts',(-2.89865056198864,-0.140751934076159,
93.4122829364753));
#14212=CARTESIAN_POINT('Ctrl Pts',(-1.4488410761114,-2.51452693783455,93.5395495709592));
#14213=CARTESIAN_POINT('Ctrl Pts',(1.33192866603113,-2.57836231230752,93.6668162054426));
#14214=CARTESIAN_POINT('Ctrl Pts',(2.88913831737708,-0.27361646611042,93.7940828399263));
#14215=CARTESIAN_POINT('Ctrl Pts',(1.7922761444701,2.28248382498065,93.9213494744098));
#14216=CARTESIAN_POINT('Ctrl Pts',(-0.951038737978436,2.74180806978394,
94.0486161088936));
#14217=CARTESIAN_POINT('Ctrl Pts',(-2.82069343799303,0.682403641351875,
94.1758827433772));
#14218=CARTESIAN_POINT('Ctrl Pts',(-2.09915236596629,-2.00388261960105,
94.3031493778608));
#14219=CARTESIAN_POINT('Ctrl Pts',(0.550749519047719,-2.84932641895892,
94.4304160123444));
#14220=CARTESIAN_POINT('Ctrl Pts',(2.69471207121477,-1.07727117779746,94.5576826468281));
#14221=CARTESIAN_POINT('Ctrl Pts',(2.36321006187575,1.68440628057551,94.6849492813116));
#14222=CARTESIAN_POINT('Ctrl Pts',(-0.13922607033149,2.89872409491546,94.8122159157953));
#14223=CARTESIAN_POINT('Ctrl Pts',(-2.51376406076365,1.45016478372299,94.9394825502789));
#14224=CARTESIAN_POINT('Ctrl Pts',(-2.57906282911108,-1.33057192336286,
95.0667491847626));
#14225=CARTESIAN_POINT('Ctrl Pts',(-0.275137668947571,-2.88899259322745,
95.1940158192461));
#14226=CARTESIAN_POINT('Ctrl Pts',(2.28154102460352,-1.79347998828841,95.3212824537299));
#14227=CARTESIAN_POINT('Ctrl Pts',(2.74230639971675,0.949600746334372,95.4485490882135));
#14228=CARTESIAN_POINT('Ctrl Pts',(0.683892160422594,2.82032291874159,95.5758157226971));
#14229=CARTESIAN_POINT('Ctrl Pts',(-2.00278524276074,2.100229102182,95.7030823571806));
#14230=CARTESIAN_POINT('Ctrl Pts',(-2.84959995676592,-0.549294827686968,
95.8303489916643));
#14231=CARTESIAN_POINT('Ctrl Pts',(-1.07872195676699,-2.69405267444053,
95.9576156261479));
#14232=CARTESIAN_POINT('Ctrl Pts',(1.68322819081122,-2.36428346291339,96.0848822606317));
#14233=CARTESIAN_POINT('Ctrl Pts',(2.89866254755287,0.138080851014796,96.2121488951151));
#14234=CARTESIAN_POINT('Ctrl Pts',(1.4517612276782,2.51222567813746,96.3394155295989));
#14235=CARTESIAN_POINT('Ctrl Pts',(-1.32976764136635,2.58134911723269,96.4666821640825));
#14236=CARTESIAN_POINT('Ctrl Pts',(-2.88770364074214,0.273366351750177,
96.593948798566));
#14237=CARTESIAN_POINT('Ctrl Pts',(-2.15978309563236,-1.42262140700734,
96.6787932215551));
#14238=CARTESIAN_POINT('Ctrl Pts',(-1.51734708719904,-1.92817607117051,
96.7212154330496));
#14239=CARTESIAN_POINT('Ctrl Pts',(1.33678351078741,-1.87092931949251,90.5741137937452));
#14240=CARTESIAN_POINT('Ctrl Pts',(1.96043134902606,-1.42536363812717,90.6165540830401));
#14241=CARTESIAN_POINT('Ctrl Pts',(2.71534063165141,0.131418296099438,90.7014165838296));
#14242=CARTESIAN_POINT('Ctrl Pts',(1.35590228238173,2.35940495037305,90.8287012961136));
#14243=CARTESIAN_POINT('Ctrl Pts',(-1.25106394636245,2.4143110549348,90.9559679305972));
#14244=CARTESIAN_POINT('Ctrl Pts',(-2.70771300429019,0.253922519790013,
91.083234565081));
#14245=CARTESIAN_POINT('Ctrl Pts',(-1.67746793173104,-2.14099352115659,
91.2105011995644));
#14246=CARTESIAN_POINT('Ctrl Pts',(0.894015126895566,-2.56849038705249,
91.3377678340482));
#14247=CARTESIAN_POINT('Ctrl Pts',(2.64409794723359,-0.636780247625117,
91.4650344685317));
#14248=CARTESIAN_POINT('Ctrl Pts',(1.9652733097387,1.880050505435,91.5923011030154));
#14249=CARTESIAN_POINT('Ctrl Pts',(-0.518955772826602,2.66972187424701,
91.7195677374989));
#14250=CARTESIAN_POINT('Ctrl Pts',(-2.5264376956473,1.00692195999112,91.8468343719827));
#14251=CARTESIAN_POINT('Ctrl Pts',(-2.21304556280866,-1.58089242218517,
91.9741010064663));
#14252=CARTESIAN_POINT('Ctrl Pts',(0.133337558970979,-2.71643041277807,
92.1013676409498));
#14253=CARTESIAN_POINT('Ctrl Pts',(2.35723000044779,-1.35655690970924,92.2286342754335));
#14254=CARTESIAN_POINT('Ctrl Pts',(2.41568259406972,1.24950324080055,92.3559009099171));
#14255=CARTESIAN_POINT('Ctrl Pts',(0.254997290569318,2.70772137397204,92.4831675444008));
#14256=CARTESIAN_POINT('Ctrl Pts',(-2.13993796864894,1.67852466731756,92.6104341788844));
#14257=CARTESIAN_POINT('Ctrl Pts',(-2.56904530714055,-0.892628589184238,
92.737700813368));
#14258=CARTESIAN_POINT('Ctrl Pts',(-0.638130327836708,-2.64377931043703,
92.8649674478516));
#14259=CARTESIAN_POINT('Ctrl Pts',(1.87899530162292,-1.96625434059751,92.9922340823353));
#14260=CARTESIAN_POINT('Ctrl Pts',(2.67000473186684,0.517546326801413,93.1195007168189));
#14261=CARTESIAN_POINT('Ctrl Pts',(1.00824673934771,2.52590933257809,93.2467673513025));
#14262=CARTESIAN_POINT('Ctrl Pts',(-1.57972487105247,2.21387641710795,93.3740339857862));
#14263=CARTESIAN_POINT('Ctrl Pts',(-2.71650141763824,-0.131907182420398,
93.5013006202697));
#14264=CARTESIAN_POINT('Ctrl Pts',(-1.35779693102744,-2.35651584944093,
93.6285672547535));
#14265=CARTESIAN_POINT('Ctrl Pts',(1.24823121383224,-2.41633985428142,93.7558338892369));
#14266=CARTESIAN_POINT('Ctrl Pts',(2.7075869157279,-0.256422601546072,93.8831005237207));
#14267=CARTESIAN_POINT('Ctrl Pts',(1.67965078340178,2.13905416113437,94.0103671582042));
#14268=CARTESIAN_POINT('Ctrl Pts',(-0.891276138568037,2.56951479634378,
94.1376337926878));
#14269=CARTESIAN_POINT('Ctrl Pts',(-2.64344306399391,0.63952188078237,94.2649004271716));
#14270=CARTESIAN_POINT('Ctrl Pts',(-1.96724312090724,-1.87796005779748,
94.3921670616551));
#14271=CARTESIAN_POINT('Ctrl Pts',(0.516140810098302,-2.67027676875468,
94.5194336961388));
#14272=CARTESIAN_POINT('Ctrl Pts',(2.52537827690404,-1.00957622144696,94.6467003306223));
#14273=CARTESIAN_POINT('Ctrl Pts',(2.21470761858861,1.5785593852068,94.7739669651061));
#14274=CARTESIAN_POINT('Ctrl Pts',(-0.130477202870647,2.71657032980812,
94.9012335995896));
#14275=CARTESIAN_POINT('Ctrl Pts',(-2.35580091102381,1.35903745779204,95.0285002340733));
#14276=CARTESIAN_POINT('Ctrl Pts',(-2.41699635110614,-1.24695972791046,
95.1557668685569));
#14277=CARTESIAN_POINT('Ctrl Pts',(-0.257848213076424,-2.70745034878043,
95.2830335030406));
#14278=CARTESIAN_POINT('Ctrl Pts',(2.13817060566391,-1.68077897852883,95.4103001375242));
#14279=CARTESIAN_POINT('Ctrl Pts',(2.56998181157724,0.889928509298448,95.5375667720078));
#14280=CARTESIAN_POINT('Ctrl Pts',(0.640916862370981,2.6430958279093,95.6648334064913));
#14281=CARTESIAN_POINT('Ctrl Pts',(-1.87693163933909,1.96825219578325,95.7921000409751));
#14282=CARTESIAN_POINT('Ctrl Pts',(-2.67053311764,-0.51477753051037,95.9193666754586));
#14283=CARTESIAN_POINT('Ctrl Pts',(-1.01093583449556,-2.52476031615517,
96.0466333099423));
#14284=CARTESIAN_POINT('Ctrl Pts',(1.5774553257673,-2.21571356786677,96.173899944426));
#14285=CARTESIAN_POINT('Ctrl Pts',(2.71651265003811,0.129403948323132,96.3011665789095));
#14286=CARTESIAN_POINT('Ctrl Pts',(1.360533582342,2.35435919927017,96.4284332133931));
#14287=CARTESIAN_POINT('Ctrl Pts',(-1.24620598642386,2.41913897050462,96.5556998478769));
#14288=CARTESIAN_POINT('Ctrl Pts',(-2.70624239315462,0.256188204194738,
96.6829664823604));
#14289=CARTESIAN_POINT('Ctrl Pts',(-2.02406385854639,-1.33322488732366,
96.7678109053495));
#14290=CARTESIAN_POINT('Ctrl Pts',(-1.42199807299214,-1.80701085514679,
96.810233116844));
#14291=CARTESIAN_POINT('Ctrl Pts',(1.24714837528162,-1.74547818868399,90.6631314775395));
#14292=CARTESIAN_POINT('Ctrl Pts',(1.82897885264073,-1.32978895320807,90.7055717668344));
#14293=CARTESIAN_POINT('Ctrl Pts',(2.53326932130208,0.122606325661629,90.7904342676238));
#14294=CARTESIAN_POINT('Ctrl Pts',(1.26498517887684,2.20120013954685,90.9177189799079));
#14295=CARTESIAN_POINT('Ctrl Pts',(-1.16717655139261,2.25242463367372,91.0449856143915));
#14296=CARTESIAN_POINT('Ctrl Pts',(-2.52615314804439,0.236896292816323,
91.1722522488752));
#14297=CARTESIAN_POINT('Ctrl Pts',(-1.56498893707412,-1.9974338177063,91.2995188833588));
#14298=CARTESIAN_POINT('Ctrl Pts',(0.83406887052957,-2.39626580316819,91.4267855178424));
#14299=CARTESIAN_POINT('Ctrl Pts',(2.46680366145111,-0.594082321354566,
91.554052152326));
#14300=CARTESIAN_POINT('Ctrl Pts',(1.83349614611961,1.75398777317319,91.6813187868096));
#14301=CARTESIAN_POINT('Ctrl Pts',(-0.484158312621983,2.49070943129734,
91.8085854212933));
#14302=CARTESIAN_POINT('Ctrl Pts',(-2.3570328642974,0.939404979418549,91.9358520557769));
#14303=CARTESIAN_POINT('Ctrl Pts',(-2.06465456508757,-1.47488909005313,
92.0631186902605));
#14304=CARTESIAN_POINT('Ctrl Pts',(0.124396896500263,-2.53428602950544,
92.1903853247442));
#14305=CARTESIAN_POINT('Ctrl Pts',(2.19917102619849,-1.26559591158063,92.3176519592278));
#14306=CARTESIAN_POINT('Ctrl Pts',(2.25370420720971,1.16572049557646,92.4449185937114));
#14307=CARTESIAN_POINT('Ctrl Pts',(0.237898997158793,2.52616095651527,92.572185228195));
#14308=CARTESIAN_POINT('Ctrl Pts',(-1.99644904299573,1.56597481553477,92.6994518626787));
#14309=CARTESIAN_POINT('Ctrl Pts',(-2.39678351428644,-0.832775304114368,
92.8267184971623));
#14310=CARTESIAN_POINT('Ctrl Pts',(-0.595341874849054,-2.4665063901578,
92.9539851316459));
#14311=CARTESIAN_POINT('Ctrl Pts',(1.75300332377717,-1.8344113960698,93.0812517661295));
#14312=CARTESIAN_POINT('Ctrl Pts',(2.49097332250947,0.482843373960504,93.2085184006132));
#14313=CARTESIAN_POINT('Ctrl Pts',(0.940640928552308,2.35653992947437,93.3357850350967));
#14314=CARTESIAN_POINT('Ctrl Pts',(-1.47379982654378,2.0654297082436,93.4630516695805));
#14315=CARTESIAN_POINT('Ctrl Pts',(-2.53435227328783,-0.123062430764635,
93.590318304064));
#14316=CARTESIAN_POINT('Ctrl Pts',(-1.26675278594347,-2.19850476104731,
93.7175849385477));
#14317=CARTESIAN_POINT('Ctrl Pts',(1.16453376163335,-2.25431739625531,93.8448515730313));
#14318=CARTESIAN_POINT('Ctrl Pts',(2.52603551407873,-0.239228736981724,
93.9721182075149));
#14319=CARTESIAN_POINT('Ctrl Pts',(1.56702542233345,1.99562449728809,94.0993848419986));
#14320=CARTESIAN_POINT('Ctrl Pts',(-0.831513539157641,2.39722152290362,
94.2266514764821));
#14321=CARTESIAN_POINT('Ctrl Pts',(-2.4661926899948,0.596640120212867,94.3539181109658));
#14322=CARTESIAN_POINT('Ctrl Pts',(-1.8353338758482,-1.75203749599391,94.4811847454494));
#14323=CARTESIAN_POINT('Ctrl Pts',(0.481532101148887,-2.49122711855045,
94.6084513799331));
#14324=CARTESIAN_POINT('Ctrl Pts',(2.3560444825933,-0.94188126509646,94.7357180144167));
#14325=CARTESIAN_POINT('Ctrl Pts',(2.06620517530148,1.47271248983809,94.8629846489003));
#14326=CARTESIAN_POINT('Ctrl Pts',(-0.121728335409802,2.53441656470078,
94.9902512833839));
#14327=CARTESIAN_POINT('Ctrl Pts',(-2.19783776128397,1.26791013186111,95.1175179178676));
#14328=CARTESIAN_POINT('Ctrl Pts',(-2.25492987310121,-1.16334753245806,
95.2447845523511));
#14329=CARTESIAN_POINT('Ctrl Pts',(-0.240558757205277,-2.52590810433341,
95.3720511868348));
#14330=CARTESIAN_POINT('Ctrl Pts',(1.99480018672429,-1.56807796876924,95.4993178213184));
#14331=CARTESIAN_POINT('Ctrl Pts',(2.39765722343773,0.830256272262522,95.6265844558021));
#14332=CARTESIAN_POINT('Ctrl Pts',(0.597941564319369,2.46586873707703,95.7538510902856));
#14333=CARTESIAN_POINT('Ctrl Pts',(-1.75107803591743,1.83627528938449,95.8811177247694));
#14334=CARTESIAN_POINT('Ctrl Pts',(-2.49146627851409,-0.480260233333773,
96.0083843592529));
#14335=CARTESIAN_POINT('Ctrl Pts',(-0.943149712224129,-2.3554679578698,
96.1356509937365));
#14336=CARTESIAN_POINT('Ctrl Pts',(1.47168246072336,-2.06714367282014,96.2629176282202));
#14337=CARTESIAN_POINT('Ctrl Pts',(2.53436275252335,0.120727045631471,96.3901842627038));
#14338=CARTESIAN_POINT('Ctrl Pts',(1.2693059370058,2.19649272040287,96.5174508971874));
#14339=CARTESIAN_POINT('Ctrl Pts',(-1.16264433148138,2.25692882377654,96.6447175316711));
#14340=CARTESIAN_POINT('Ctrl Pts',(-2.52478114556709,0.239010056639298,
96.7719841661547));
#14341=CARTESIAN_POINT('Ctrl Pts',(-1.88834462146043,-1.24382836763997,
96.8568285891438));
#14342=CARTESIAN_POINT('Ctrl Pts',(-1.32664905878525,-1.68584563912308,
96.8992508006383));
#14343=CARTESIAN_POINT('Ctrl Pts',(1.15751323977584,-1.62002705787548,90.7521491613338));
#14344=CARTESIAN_POINT('Ctrl Pts',(1.69752635625542,-1.23421426828898,90.7945894506287));
#14345=CARTESIAN_POINT('Ctrl Pts',(2.35119801095275,0.113794355223823,90.8794519514181));
#14346=CARTESIAN_POINT('Ctrl Pts',(1.17406807537195,2.04299532872065,91.0067366637022));
#14347=CARTESIAN_POINT('Ctrl Pts',(-1.08328915642277,2.09053821241265,91.1340032981858));
#14348=CARTESIAN_POINT('Ctrl Pts',(-2.34459329179859,0.219870065842631,
91.2612699326695));
#14349=CARTESIAN_POINT('Ctrl Pts',(-1.45250994241719,-1.85387411425601,
91.3885365671531));
#14350=CARTESIAN_POINT('Ctrl Pts',(0.774122614163573,-2.2240412192839,91.5158032016367));
#14351=CARTESIAN_POINT('Ctrl Pts',(2.28950937566864,-0.551384395084015,
91.6430698361204));
#14352=CARTESIAN_POINT('Ctrl Pts',(1.70171898250053,1.6279250409114,91.7703364706039));
#14353=CARTESIAN_POINT('Ctrl Pts',(-0.449360852417364,2.31169698834768,
91.8976031050876));
#14354=CARTESIAN_POINT('Ctrl Pts',(-2.18762803294751,0.871887998845985,
92.0248697395712));
#14355=CARTESIAN_POINT('Ctrl Pts',(-1.9162635673665,-1.3688857579211,92.1521363740549));
#14356=CARTESIAN_POINT('Ctrl Pts',(0.115456234029549,-2.3521416462328,92.2794030085384));
#14357=CARTESIAN_POINT('Ctrl Pts',(2.04111205194919,-1.17463491345201,92.4066696430221));
#14358=CARTESIAN_POINT('Ctrl Pts',(2.0917258203497,1.08193775035237,92.5339362775058));
#14359=CARTESIAN_POINT('Ctrl Pts',(0.220800703748267,2.3446005390585,92.6612029119892));
#14360=CARTESIAN_POINT('Ctrl Pts',(-1.85296011734251,1.45342496375197,92.7884695464731));
#14361=CARTESIAN_POINT('Ctrl Pts',(-2.22452172143234,-0.772922019044498,
92.9157361809566));
#14362=CARTESIAN_POINT('Ctrl Pts',(-0.552553421861399,-2.28923346987856,
93.0430028154402));
#14363=CARTESIAN_POINT('Ctrl Pts',(1.62701134593142,-1.7025684515421,93.1702694499238));
#14364=CARTESIAN_POINT('Ctrl Pts',(2.31194191315208,0.448140421119597,93.2975360844075));
#14365=CARTESIAN_POINT('Ctrl Pts',(0.873035117756911,2.18717052637064,93.4248027188911));
#14366=CARTESIAN_POINT('Ctrl Pts',(-1.36787478203509,1.91698299937924,93.5520693533747));
#14367=CARTESIAN_POINT('Ctrl Pts',(-2.35220312893742,-0.114217679108873,
93.6793359878583));
#14368=CARTESIAN_POINT('Ctrl Pts',(-1.1757086408595,-2.04049367265369,93.806602622342));
#14369=CARTESIAN_POINT('Ctrl Pts',(1.08083630943445,-2.0922949382292,93.9338692568256));
#14370=CARTESIAN_POINT('Ctrl Pts',(2.34448411242956,-0.222034872417374,
94.0611358913091));
#14371=CARTESIAN_POINT('Ctrl Pts',(1.45440006126512,1.85219483344182,94.188402525793));
#14372=CARTESIAN_POINT('Ctrl Pts',(-0.771750939747243,2.22492824946345,
94.3156691602764));
#14373=CARTESIAN_POINT('Ctrl Pts',(-2.28894231599568,0.553758359643362,
94.4429357947601));
#14374=CARTESIAN_POINT('Ctrl Pts',(-1.70342463078915,-1.62611493419034,
94.5702024292437));
#14375=CARTESIAN_POINT('Ctrl Pts',(0.446923392199468,-2.31217746834622,
94.6974690637273));
#14376=CARTESIAN_POINT('Ctrl Pts',(2.18671068828257,-0.87418630874596,94.824735698211));
#14377=CARTESIAN_POINT('Ctrl Pts',(1.91770273201434,1.36686559446937,94.9520023326946));
#14378=CARTESIAN_POINT('Ctrl Pts',(-0.112979467948959,2.35226279959343,
95.0792689671782));
#14379=CARTESIAN_POINT('Ctrl Pts',(-2.03987461154412,1.17678280593016,95.2065356016618));
#14380=CARTESIAN_POINT('Ctrl Pts',(-2.09286339509628,-1.07973533700565,
95.3338022361456));
#14381=CARTESIAN_POINT('Ctrl Pts',(-0.223269301334131,-2.34436585988639,
95.4610688706291));
#14382=CARTESIAN_POINT('Ctrl Pts',(1.85142976778467,-1.45537695900965,95.5883355051127));
#14383=CARTESIAN_POINT('Ctrl Pts',(2.22533263529822,0.770584035226599,95.7156021395964));
#14384=CARTESIAN_POINT('Ctrl Pts',(0.554966266267755,2.28864164624474,95.84286877408));
#14385=CARTESIAN_POINT('Ctrl Pts',(-1.62522443249577,1.70429838298573,95.9701354085636));
#14386=CARTESIAN_POINT('Ctrl Pts',(-2.31239943938818,-0.445742936157174,
96.0974020430472));
#14387=CARTESIAN_POINT('Ctrl Pts',(-0.875363589952698,-2.18617559958444,
96.2246686775309));
#14388=CARTESIAN_POINT('Ctrl Pts',(1.36590959567943,-1.91857377777351,96.3519353120145));
#14389=CARTESIAN_POINT('Ctrl Pts',(2.3522128550086,0.112050142939805,96.4792019464981));
#14390=CARTESIAN_POINT('Ctrl Pts',(1.17807829166959,2.03862624153558,96.6064685809818));
#14391=CARTESIAN_POINT('Ctrl Pts',(-1.0790826765389,2.09471867704846,96.7337352154654));
#14392=CARTESIAN_POINT('Ctrl Pts',(-2.34331989797958,0.221831909083859,
96.861001849949));
#14393=CARTESIAN_POINT('Ctrl Pts',(-1.75262538437446,-1.15443184795629,
96.9458462729381));
#14394=CARTESIAN_POINT('Ctrl Pts',(-1.23130004457835,-1.56468042309936,
96.9882684844326));
#14395=CARTESIAN_POINT('',(-0.793252505200376,1.83204963892414,96.723977388184));
#14396=CARTESIAN_POINT('Ctrl Pts',(-0.794009102248012,1.83356035954796,
96.7230113585668));
#14397=CARTESIAN_POINT('Ctrl Pts',(-0.837291874002563,1.82051106939911,
96.7230113585668));
#14398=CARTESIAN_POINT('Ctrl Pts',(-0.880023176065944,1.8059130308115,96.7230113585668));
#14399=CARTESIAN_POINT('Ctrl Pts',(-0.922118158570995,1.7897642254726,96.7230113585668));
#14400=CARTESIAN_POINT('Ctrl Pts',(-0.989542432506282,1.76389839990142,
96.7230113585668));
#14401=CARTESIAN_POINT('Ctrl Pts',(-1.05533499621115,1.73405720162925,96.7230113585668));
#14402=CARTESIAN_POINT('Ctrl Pts',(-1.11933937792182,1.70056771355782,96.7230113585668));
#14403=CARTESIAN_POINT('Ctrl Pts',(-1.17096240512104,1.67355661357696,96.7230113585668));
#14404=CARTESIAN_POINT('Ctrl Pts',(-1.2214222453498,1.64417097646139,96.7230113585668));
#14405=CARTESIAN_POINT('Ctrl Pts',(-1.27063140042659,1.612558416562,96.7230113585668));
#14406=CARTESIAN_POINT('Ctrl Pts',(-1.28395910376886,1.60399653779023,96.7230113585668));
#14407=CARTESIAN_POINT('Ctrl Pts',(-1.29718718705757,1.59527619216679,96.7230113585668));
#14408=CARTESIAN_POINT('Ctrl Pts',(-1.31031056320797,1.58640318349424,96.7230113585668));
#14409=CARTESIAN_POINT('Ctrl Pts',(-1.37255435913609,1.54431875836207,96.7230113585668));
#14410=CARTESIAN_POINT('Ctrl Pts',(-1.43246940936956,1.4987878264592,96.7230113585668));
#14411=CARTESIAN_POINT('Ctrl Pts',(-1.48988552335752,1.45015309019523,96.7230113585668));
#14412=CARTESIAN_POINT('Ctrl Pts',(-1.53653455176071,1.41063869195792,96.7230113585668));
#14413=CARTESIAN_POINT('Ctrl Pts',(-1.58153400798001,1.36907421455917,96.7230113585668));
#14414=CARTESIAN_POINT('Ctrl Pts',(-1.62478412958448,1.32561968798594,96.7230113585668));
#14415=CARTESIAN_POINT('Ctrl Pts',(-1.64255840351002,1.30776141083055,96.7230113585668));
#14416=CARTESIAN_POINT('Ctrl Pts',(-1.66003711651052,1.28958369174573,96.7230113585668));
#14417=CARTESIAN_POINT('Ctrl Pts',(-1.67721281325249,1.27109674069572,96.7230113585668));
#14418=CARTESIAN_POINT('Ctrl Pts',(-1.68809273408154,1.25938620767827,96.7230113585668));
#14419=CARTESIAN_POINT('Ctrl Pts',(-1.69885185685385,1.24755050758685,96.7230113585668));
#14420=CARTESIAN_POINT('Ctrl Pts',(-1.70947475987798,1.23560780147555,96.7230113585668));
#14421=CARTESIAN_POINT('Ctrl Pts',(-1.76143601470801,1.1771908137463,96.7230113585668));
#14422=CARTESIAN_POINT('Ctrl Pts',(-1.81021688338235,1.11613601970109,96.7230113585668));
#14423=CARTESIAN_POINT('Ctrl Pts',(-1.85564060628833,1.05279736816488,96.7230113585668));
#14424=CARTESIAN_POINT('Ctrl Pts',(-1.90162151964286,0.988681772569438,
96.7230113585668));
#14425=CARTESIAN_POINT('Ctrl Pts',(-1.94416322520855,0.922225295514363,
96.7230113585668));
#14426=CARTESIAN_POINT('Ctrl Pts',(-1.98305655594857,0.853748149314053,
96.7230113585668));
#14427=CARTESIAN_POINT('Ctrl Pts',(-2.02172591850317,0.785665330415768,
96.7230113585668));
#14428=CARTESIAN_POINT('Ctrl Pts',(-2.05678954190754,0.715584254543018,
96.7230113585668));
#14429=CARTESIAN_POINT('Ctrl Pts',(-2.08800503716774,0.643784571834216,
96.7230113585668));
#14430=CARTESIAN_POINT('Ctrl Pts',(-2.09678381022876,0.623592256604256,
96.7230113585668));
#14431=CARTESIAN_POINT('Ctrl Pts',(-2.10525796886676,0.603263841203811,
96.7230113585668));
#14432=CARTESIAN_POINT('Ctrl Pts',(-2.1134214676846,0.582805175485435,96.7230113585668));
#14433=CARTESIAN_POINT('Ctrl Pts',(-2.11827851823285,0.570632848917964,
96.7230113585668));
#14434=CARTESIAN_POINT('Ctrl Pts',(-2.12302631749701,0.558412486391,96.7230113585668));
#14435=CARTESIAN_POINT('Ctrl Pts',(-2.12766122540615,0.546151436333585,
96.7230113585668));
#14436=CARTESIAN_POINT('Ctrl Pts',(-2.15633033981201,0.470310998136579,
96.7230113585668));
#14437=CARTESIAN_POINT('Ctrl Pts',(-2.1805880672175,0.393172356210161,96.7230113585668));
#14438=CARTESIAN_POINT('Ctrl Pts',(-2.20023085075779,0.315077935502425,
96.7230113585668));
#14439=CARTESIAN_POINT('Ctrl Pts',(-2.20877013194232,0.281128051770403,
96.7230113585668));
#14440=CARTESIAN_POINT('Ctrl Pts',(-2.21643679729787,0.246997034801529,
96.7230113585668));
#14441=CARTESIAN_POINT('Ctrl Pts',(-2.2232118307638,0.212710970602204,96.7230113585668));
#14442=CARTESIAN_POINT('Ctrl Pts',(-2.2384123422071,0.135786522357324,96.7230113585668));
#14443=CARTESIAN_POINT('Ctrl Pts',(-2.24912823491718,0.0580828721013101,
96.7230113585667));
#14444=CARTESIAN_POINT('Ctrl Pts',(-2.25553969589224,-0.0200953176490006,
96.7230113585667));
#14445=CARTESIAN_POINT('Ctrl Pts',(-2.2619511568673,-0.0982735073993113,
96.7230113585667));
#14446=CARTESIAN_POINT('Ctrl Pts',(-2.26405806090902,-0.176927046626794,
96.7230113585667));
#14447=CARTESIAN_POINT('Ctrl Pts',(-2.26198999100256,-0.255764556751951,
96.7230113585667));
#14448=CARTESIAN_POINT('Ctrl Pts',(-2.26164030555424,-0.26909502009201,
96.7230113585667));
#14449=CARTESIAN_POINT('Ctrl Pts',(-2.26117114012459,-0.28243075742817,
96.7230113585667));
#14450=CARTESIAN_POINT('Ctrl Pts',(-2.26058298212319,-0.295770371599199,
96.7230113585667));
#14451=CARTESIAN_POINT('Ctrl Pts',(-2.26002859528514,-0.308344044835706,
96.7230113585667));
#14452=CARTESIAN_POINT('Ctrl Pts',(-2.25936891052518,-0.320911461615806,
96.7230113585667));
#14453=CARTESIAN_POINT('Ctrl Pts',(-2.25860486758928,-0.333470453701026,
96.7230113585667));
#14454=CARTESIAN_POINT('Ctrl Pts',(-2.25370545505801,-0.414004780126182,
96.7230113585667));
#14455=CARTESIAN_POINT('Ctrl Pts',(-2.2445184297719,-0.494203504147783,
96.7230113585667));
#14456=CARTESIAN_POINT('Ctrl Pts',(-2.23125141378542,-0.573747205190449,
96.7230113585667));
#14457=CARTESIAN_POINT('Ctrl Pts',(-2.21758819715782,-0.65566636619959,
96.7230113585667));
#14458=CARTESIAN_POINT('Ctrl Pts',(-2.199597743887,-0.736891642756019,96.7230113585667));
#14459=CARTESIAN_POINT('Ctrl Pts',(-2.17745214020847,-0.817087333965471,
96.7230113585667));
#14460=CARTESIAN_POINT('Ctrl Pts',(-2.15530653652994,-0.897283025174922,
96.7230113585667));
#14461=CARTESIAN_POINT('Ctrl Pts',(-2.1290055920952,-0.976450102162561,
96.7230113585667));
#14462=CARTESIAN_POINT('Ctrl Pts',(-2.09866874566655,-1.05425199061378,
96.7230113585667));
#14463=CARTESIAN_POINT('Ctrl Pts',(-2.08661076762519,-1.08517588590817,
96.7230113585667));
#14464=CARTESIAN_POINT('Ctrl Pts',(-2.07391462100506,-1.11588401593709,
96.7230113585667));
#14465=CARTESIAN_POINT('Ctrl Pts',(-2.06058559778188,-1.14635467735089,
96.7230113585667));
#14466=CARTESIAN_POINT('Ctrl Pts',(-2.05390436829635,-1.16162822576271,
96.7230113585667));
#14467=CARTESIAN_POINT('Ctrl Pts',(-2.04706257850103,-1.17684515372061,
96.7230113585667));
#14468=CARTESIAN_POINT('Ctrl Pts',(-2.04007193789771,-1.19197928395999,
96.7230113585667));
#14469=CARTESIAN_POINT('Ctrl Pts',(-2.00405444114075,-1.26995403874251,
96.7230113585667));
#14470=CARTESIAN_POINT('Ctrl Pts',(-1.96403813188458,-1.34585382007019,
96.7230113585667));
#14471=CARTESIAN_POINT('Ctrl Pts',(-1.92021044960232,-1.41933358024217,
96.7230113585667));
#14472=CARTESIAN_POINT('Ctrl Pts',(-1.87632015444256,-1.49291831469027,
96.7230113585667));
#14473=CARTESIAN_POINT('Ctrl Pts',(-1.82860736272488,-1.56407711696169,
96.7230113585667));
#14474=CARTESIAN_POINT('Ctrl Pts',(-1.77720857262822,-1.632456840965,96.7230113585667));
#14475=CARTESIAN_POINT('Ctrl Pts',(-1.72691027409469,-1.6993724972497,96.7230113585667));
#14476=CARTESIAN_POINT('Ctrl Pts',(-1.67308174783659,-1.7636276913924,96.7230113585667));
#14477=CARTESIAN_POINT('Ctrl Pts',(-1.61580616688792,-1.82487124435851,
96.7230113585667));
#14478=CARTESIAN_POINT('Ctrl Pts',(-1.58344350848759,-1.85947594239974,
96.7230113585667));
#14479=CARTESIAN_POINT('Ctrl Pts',(-1.54997954742544,-1.89311869319316,
96.7230113585666));
#14480=CARTESIAN_POINT('Ctrl Pts',(-1.51542342753583,-1.92573157144902,
96.7230113585666));
#14481=CARTESIAN_POINT('Ctrl Pts',(-0.766343857929314,1.84166898597821,
96.7230113585667));
#14482=CARTESIAN_POINT('Ctrl Pts',(-0.775119863224321,1.83801716917172,
96.7233333684391));
#14483=CARTESIAN_POINT('Ctrl Pts',(-0.783869765361946,1.83430262156666,
96.7236553783116));
#14484=CARTESIAN_POINT('Ctrl Pts',(-0.792592670269147,1.83052572271892,
96.723977388184));
#14485=CARTESIAN_POINT('Ctrl Pts',(1.11860366144128,2.18029266352253,90.7500736540522));
#14486=CARTESIAN_POINT('Ctrl Pts',(1.10424245208046,2.18748324778742,90.7500736540522));
#14487=CARTESIAN_POINT('Ctrl Pts',(1.08988124271963,2.19467383205231,90.7500736540522));
#14488=CARTESIAN_POINT('Ctrl Pts',(1.07552003335881,2.2018644163172,90.7500736540522));
#14489=CARTESIAN_POINT('Origin',(0.,0.,88.2780718176998));
#14490=CARTESIAN_POINT('',(-1.77103530981268,-2.16889272333904E-16,88.2780718176998));
#14491=CARTESIAN_POINT('Origin',(-6.60753780880871,-8.0919000278027E-16,
88.2780718176998));
#14492=CARTESIAN_POINT('Origin',(0.,0.,88.2780718176998));
#14493=CARTESIAN_POINT('Origin',(3.86373699625103,0.,96.7230113585667));
#14494=CARTESIAN_POINT('',(-3.86373699625103,-4.73171314520603E-16,96.7230113585667));
#14495=CARTESIAN_POINT('Origin',(0.,0.,96.7230113585667));
#14496=CARTESIAN_POINT('Origin',(0.,0.,98.1470603273161));
#14497=CARTESIAN_POINT('',(-3.86373699625103,-4.73171314520603E-16,99.5711092960655));
#14498=CARTESIAN_POINT('Origin',(0.,0.,99.5711092960655));
#14499=CARTESIAN_POINT('',(-3.86373699625103,-4.73171314520603E-16,98.1470603273161));
#14500=CARTESIAN_POINT('Origin',(0.,0.,99.6988479078803));
#14501=CARTESIAN_POINT('',(-3.53729387716894,-4.33193562431847E-16,99.826586519695));
#14502=CARTESIAN_POINT('',(-3.70051543670999,4.53182438476226E-16,99.6988479078803));
#14503=CARTESIAN_POINT('Origin',(0.,0.,99.826586519695));
#14504=CARTESIAN_POINT('Origin',(0.684464879973279,0.,99.826586519695));
#14505=CARTESIAN_POINT('',(-0.684464879973279,-8.38227724388054E-17,99.826586519695));
#14506=CARTESIAN_POINT('Origin',(0.,0.,99.826586519695));
#14507=CARTESIAN_POINT('Origin',(0.,0.,98.9134919982045));
#14508=CARTESIAN_POINT('',(-0.684464879973279,-8.38227724388054E-17,98.000397476714));
#14509=CARTESIAN_POINT('Origin',(0.,0.,98.000397476714));
#14510=CARTESIAN_POINT('',(-0.684464879973279,-8.38227724388053E-17,98.9134919982045));
#14511=CARTESIAN_POINT('Origin',(0.,0.,98.000397476714));
#14512=CARTESIAN_POINT('Origin',(1.77103530981268,0.,87.0039956821063));
#14513=CARTESIAN_POINT('',(-1.77103530981268,-2.16889272333904E-16,87.0039956821063));
#14514=CARTESIAN_POINT('Origin',(0.,0.,87.0039956821063));
#14515=CARTESIAN_POINT('Origin',(0.,0.,87.6410337499031));
#14516=CARTESIAN_POINT('',(-1.77103530981268,-2.16889272333904E-16,87.6410337499031));
#14517=CARTESIAN_POINT('',(0.,0.,0.));
#14518=CARTESIAN_POINT('',(0.,0.,0.));
#14519=CARTESIAN_POINT('',(0.,0.,0.));
#14520=CARTESIAN_POINT('',(0.,0.,0.));
#14521=CARTESIAN_POINT('',(0.,0.,0.));
#14522=CARTESIAN_POINT('',(0.,0.,0.));
#14523=CARTESIAN_POINT('',(0.,0.,0.));
#14524=CARTESIAN_POINT('',(0.,0.,0.));
#14525=UNCERTAINTY_MEASURE_WITH_UNIT(LENGTH_MEASURE(0.01),#14545,
'DISTANCE_ACCURACY_VALUE',
'Maximum model space distance between geometric entities at asserted c
onnectivities');
#14526=UNCERTAINTY_MEASURE_WITH_UNIT(LENGTH_MEASURE(0.01),#14545,
'DISTANCE_ACCURACY_VALUE',
'Maximum model space distance between geometric entities at asserted c
onnectivities');
#14527=UNCERTAINTY_MEASURE_WITH_UNIT(LENGTH_MEASURE(0.01),#14545,
'DISTANCE_ACCURACY_VALUE',
'Maximum model space distance between geometric entities at asserted c
onnectivities');
#14528=UNCERTAINTY_MEASURE_WITH_UNIT(LENGTH_MEASURE(0.01),#14545,
'DISTANCE_ACCURACY_VALUE',
'Maximum model space distance between geometric entities at asserted c
onnectivities');
#14529=UNCERTAINTY_MEASURE_WITH_UNIT(LENGTH_MEASURE(0.01),#14545,
'DISTANCE_ACCURACY_VALUE',
'Maximum model space distance between geometric entities at asserted c
onnectivities');
#14530=UNCERTAINTY_MEASURE_WITH_UNIT(LENGTH_MEASURE(0.01),#14545,
'DISTANCE_ACCURACY_VALUE',
'Maximum model space distance between geometric entities at asserted c
onnectivities');
#14531=UNCERTAINTY_MEASURE_WITH_UNIT(LENGTH_MEASURE(0.01),#14545,
'DISTANCE_ACCURACY_VALUE',
'Maximum model space distance between geometric entities at asserted c
onnectivities');
#14532=UNCERTAINTY_MEASURE_WITH_UNIT(LENGTH_MEASURE(0.01),#14545,
'DISTANCE_ACCURACY_VALUE',
'Maximum model space distance between geometric entities at asserted c
onnectivities');
#14533=UNCERTAINTY_MEASURE_WITH_UNIT(LENGTH_MEASURE(0.01),#14545,
'DISTANCE_ACCURACY_VALUE',
'Maximum model space distance between geometric entities at asserted c
onnectivities');
#14534=UNCERTAINTY_MEASURE_WITH_UNIT(LENGTH_MEASURE(0.01),#14545,
'DISTANCE_ACCURACY_VALUE',
'Maximum model space distance between geometric entities at asserted c
onnectivities');
#14535=(
GEOMETRIC_REPRESENTATION_CONTEXT(3)
GLOBAL_UNCERTAINTY_ASSIGNED_CONTEXT((#14525))
GLOBAL_UNIT_ASSIGNED_CONTEXT((#14545,#14547,#14548))
REPRESENTATION_CONTEXT('','3D')
);
#14536=(
GEOMETRIC_REPRESENTATION_CONTEXT(3)
GLOBAL_UNCERTAINTY_ASSIGNED_CONTEXT((#14526))
GLOBAL_UNIT_ASSIGNED_CONTEXT((#14545,#14547,#14548))
REPRESENTATION_CONTEXT('','3D')
);
#14537=(
GEOMETRIC_REPRESENTATION_CONTEXT(3)
GLOBAL_UNCERTAINTY_ASSIGNED_CONTEXT((#14527))
GLOBAL_UNIT_ASSIGNED_CONTEXT((#14545,#14547,#14548))
REPRESENTATION_CONTEXT('','3D')
);
#14538=(
GEOMETRIC_REPRESENTATION_CONTEXT(3)
GLOBAL_UNCERTAINTY_ASSIGNED_CONTEXT((#14528))
GLOBAL_UNIT_ASSIGNED_CONTEXT((#14545,#14547,#14548))
REPRESENTATION_CONTEXT('','3D')
);
#14539=(
GEOMETRIC_REPRESENTATION_CONTEXT(3)
GLOBAL_UNCERTAINTY_ASSIGNED_CONTEXT((#14529))
GLOBAL_UNIT_ASSIGNED_CONTEXT((#14545,#14547,#14548))
REPRESENTATION_CONTEXT('','3D')
);
#14540=(
GEOMETRIC_REPRESENTATION_CONTEXT(3)
GLOBAL_UNCERTAINTY_ASSIGNED_CONTEXT((#14530))
GLOBAL_UNIT_ASSIGNED_CONTEXT((#14545,#14547,#14548))
REPRESENTATION_CONTEXT('','3D')
);
#14541=(
GEOMETRIC_REPRESENTATION_CONTEXT(3)
GLOBAL_UNCERTAINTY_ASSIGNED_CONTEXT((#14531))
GLOBAL_UNIT_ASSIGNED_CONTEXT((#14545,#14547,#14548))
REPRESENTATION_CONTEXT('','3D')
);
#14542=(
GEOMETRIC_REPRESENTATION_CONTEXT(3)
GLOBAL_UNCERTAINTY_ASSIGNED_CONTEXT((#14532))
GLOBAL_UNIT_ASSIGNED_CONTEXT((#14545,#14547,#14548))
REPRESENTATION_CONTEXT('','3D')
);
#14543=(
GEOMETRIC_REPRESENTATION_CONTEXT(3)
GLOBAL_UNCERTAINTY_ASSIGNED_CONTEXT((#14533))
GLOBAL_UNIT_ASSIGNED_CONTEXT((#14545,#14547,#14548))
REPRESENTATION_CONTEXT('','3D')
);
#14544=(
GEOMETRIC_REPRESENTATION_CONTEXT(3)
GLOBAL_UNCERTAINTY_ASSIGNED_CONTEXT((#14534))
GLOBAL_UNIT_ASSIGNED_CONTEXT((#14545,#14547,#14548))
REPRESENTATION_CONTEXT('','3D')
);
#14545=(
LENGTH_UNIT()
NAMED_UNIT(*)
SI_UNIT(.MILLI.,.METRE.)
);
#14546=(
LENGTH_UNIT()
NAMED_UNIT(*)
SI_UNIT($,.METRE.)
);
#14547=(
NAMED_UNIT(*)
PLANE_ANGLE_UNIT()
SI_UNIT($,.RADIAN.)
);
#14548=(
NAMED_UNIT(*)
SI_UNIT($,.STERADIAN.)
SOLID_ANGLE_UNIT()
);
#14549=SHAPE_DEFINITION_REPRESENTATION(#14558,#14575);
#14550=SHAPE_DEFINITION_REPRESENTATION(#14559,#14576);
#14551=SHAPE_DEFINITION_REPRESENTATION(#14560,#14577);
#14552=SHAPE_DEFINITION_REPRESENTATION(#14561,#14578);
#14553=SHAPE_DEFINITION_REPRESENTATION(#14562,#14579);
#14554=SHAPE_DEFINITION_REPRESENTATION(#14563,#14580);
#14555=SHAPE_DEFINITION_REPRESENTATION(#14564,#14581);
#14556=SHAPE_DEFINITION_REPRESENTATION(#14565,#14582);
#14557=SHAPE_DEFINITION_REPRESENTATION(#14566,#14583);
#14558=PRODUCT_DEFINITION_SHAPE('',$,#14585);
#14559=PRODUCT_DEFINITION_SHAPE('',$,#14586);
#14560=PRODUCT_DEFINITION_SHAPE('',$,#14587);
#14561=PRODUCT_DEFINITION_SHAPE('',$,#14588);
#14562=PRODUCT_DEFINITION_SHAPE('',$,#14589);
#14563=PRODUCT_DEFINITION_SHAPE('',$,#14590);
#14564=PRODUCT_DEFINITION_SHAPE('',$,#14591);
#14565=PRODUCT_DEFINITION_SHAPE('',$,#14592);
#14566=PRODUCT_DEFINITION_SHAPE('',$,#14593);
#14567=PRODUCT_DEFINITION_SHAPE($,$,#35);
#14568=PRODUCT_DEFINITION_SHAPE($,$,#36);
#14569=PRODUCT_DEFINITION_SHAPE($,$,#37);
#14570=PRODUCT_DEFINITION_SHAPE($,$,#38);
#14571=PRODUCT_DEFINITION_SHAPE($,$,#39);
#14572=PRODUCT_DEFINITION_SHAPE($,$,#40);
#14573=PRODUCT_DEFINITION_SHAPE($,$,#41);
#14574=PRODUCT_DEFINITION_SHAPE($,$,#42);
#14575=SHAPE_REPRESENTATION('',(#1923,#2120,#2121,#2122,#2123,#2124,#2125,
#2126,#2127),#14535);
#14576=SHAPE_REPRESENTATION('',(#1924),#14536);
#14577=SHAPE_REPRESENTATION('',(#1933),#14537);
#14578=SHAPE_REPRESENTATION('',(#1966),#14538);
#14579=SHAPE_REPRESENTATION('',(#1982),#14539);
#14580=SHAPE_REPRESENTATION('',(#1991),#14540);
#14581=SHAPE_REPRESENTATION('',(#2004),#14541);
#14582=SHAPE_REPRESENTATION('',(#2047),#14542);
#14583=SHAPE_REPRESENTATION('',(#2086),#14543);
#14584=PRODUCT_DEFINITION_CONTEXT('part definition',#14613,'design');
#14585=PRODUCT_DEFINITION('BR-113','BR-113',#14594,#14584);
#14586=PRODUCT_DEFINITION('Tube','Tube',#14595,#14584);
#14587=PRODUCT_DEFINITION('Piston','Piston',#14596,#14584);
#14588=PRODUCT_DEFINITION('Shaft','Shaft',#14597,#14584);
#14589=PRODUCT_DEFINITION('Disc','Disc',#14598,#14584);
#14590=PRODUCT_DEFINITION('Cover','Cover',#14599,#14584);
#14591=PRODUCT_DEFINITION('Screw_01','Screw_01',#14600,#14584);
#14592=PRODUCT_DEFINITION('Top_Part','Top_Part',#14601,#14584);
#14593=PRODUCT_DEFINITION('Screw_02','Screw_02',#14602,#14584);
#14594=PRODUCT_DEFINITION_FORMATION('',$,#14615);
#14595=PRODUCT_DEFINITION_FORMATION('',$,#14616);
#14596=PRODUCT_DEFINITION_FORMATION('',$,#14617);
#14597=PRODUCT_DEFINITION_FORMATION('',$,#14618);
#14598=PRODUCT_DEFINITION_FORMATION('',$,#14619);
#14599=PRODUCT_DEFINITION_FORMATION('',$,#14620);
#14600=PRODUCT_DEFINITION_FORMATION('',$,#14621);
#14601=PRODUCT_DEFINITION_FORMATION('',$,#14622);
#14602=PRODUCT_DEFINITION_FORMATION('',$,#14623);
#14603=PRODUCT_RELATED_PRODUCT_CATEGORY('BR-113','BR-113',(#14615));
#14604=PRODUCT_RELATED_PRODUCT_CATEGORY('Tube','Tube',(#14616));
#14605=PRODUCT_RELATED_PRODUCT_CATEGORY('Piston','Piston',(#14617));
#14606=PRODUCT_RELATED_PRODUCT_CATEGORY('Shaft','Shaft',(#14618));
#14607=PRODUCT_RELATED_PRODUCT_CATEGORY('Disc','Disc',(#14619));
#14608=PRODUCT_RELATED_PRODUCT_CATEGORY('Cover','Cover',(#14620));
#14609=PRODUCT_RELATED_PRODUCT_CATEGORY('Screw_01','Screw_01',(#14621));
#14610=PRODUCT_RELATED_PRODUCT_CATEGORY('Top_Part','Top_Part',(#14622));
#14611=PRODUCT_RELATED_PRODUCT_CATEGORY('Screw_02','Screw_02',(#14623));
#14612=APPLICATION_PROTOCOL_DEFINITION('international standard',
'automotive_design',2009,#14613);
#14613=APPLICATION_CONTEXT(
'Core Data for Automotive Mechanical Design Process');
#14614=PRODUCT_CONTEXT('part definition',#14613,'mechanical');
#14615=PRODUCT('BR-113','BR-113',$,(#14614));
#14616=PRODUCT('Tube','Tube',$,(#14614));
#14617=PRODUCT('Piston','Piston',$,(#14614));
#14618=PRODUCT('Shaft','Shaft',$,(#14614));
#14619=PRODUCT('Disc','Disc',$,(#14614));
#14620=PRODUCT('Cover','Cover',$,(#14614));
#14621=PRODUCT('Screw_01','Screw_01',$,(#14614));
#14622=PRODUCT('Top_Part','Top_Part',$,(#14614));
#14623=PRODUCT('Screw_02','Screw_02',$,(#14614));
#14624=PRESENTATION_STYLE_ASSIGNMENT((#14628));
#14625=PRESENTATION_STYLE_ASSIGNMENT((#14629));
#14626=PRESENTATION_STYLE_ASSIGNMENT((#14630));
#14627=PRESENTATION_STYLE_ASSIGNMENT((#14631));
#14628=SURFACE_STYLE_USAGE(.BOTH.,#14632);
#14629=SURFACE_STYLE_USAGE(.BOTH.,#14633);
#14630=SURFACE_STYLE_USAGE(.BOTH.,#14634);
#14631=SURFACE_STYLE_USAGE(.BOTH.,#14635);
#14632=SURFACE_SIDE_STYLE('',(#14636));
#14633=SURFACE_SIDE_STYLE('',(#14637));
#14634=SURFACE_SIDE_STYLE('',(#14638));
#14635=SURFACE_SIDE_STYLE('',(#14639));
#14636=SURFACE_STYLE_FILL_AREA(#14640);
#14637=SURFACE_STYLE_FILL_AREA(#14641);
#14638=SURFACE_STYLE_FILL_AREA(#14642);
#14639=SURFACE_STYLE_FILL_AREA(#14643);
#14640=FILL_AREA_STYLE('Steel - Satin',(#14644));
#14641=FILL_AREA_STYLE('Opaque(246,246,243)',(#14645));
#14642=FILL_AREA_STYLE('Opaque(39,39,39)',(#14646));
#14643=FILL_AREA_STYLE('Opaque(203,203,203)',(#14647));
#14644=FILL_AREA_STYLE_COLOUR('Steel - Satin',#14648);
#14645=FILL_AREA_STYLE_COLOUR('Opaque(246,246,243)',#14649);
#14646=FILL_AREA_STYLE_COLOUR('Opaque(39,39,39)',#14650);
#14647=FILL_AREA_STYLE_COLOUR('Opaque(203,203,203)',#14651);
#14648=COLOUR_RGB('Steel - Satin', 0.09019608, 0.27058824, 0.51372549);
#14649=COLOUR_RGB('Opaque(246,246,243)', 0.09019608, 0.27058824, 0.51372549);
#14650=COLOUR_RGB('Opaque(39,39,39)', 0.66274510, 0.83137255, 0.94901961);
#14651=COLOUR_RGB('Opaque(203,203,203)', 0.31764706, 0.68627451, 0.89019608);
ENDSEC;
END-ISO-10303-21;
